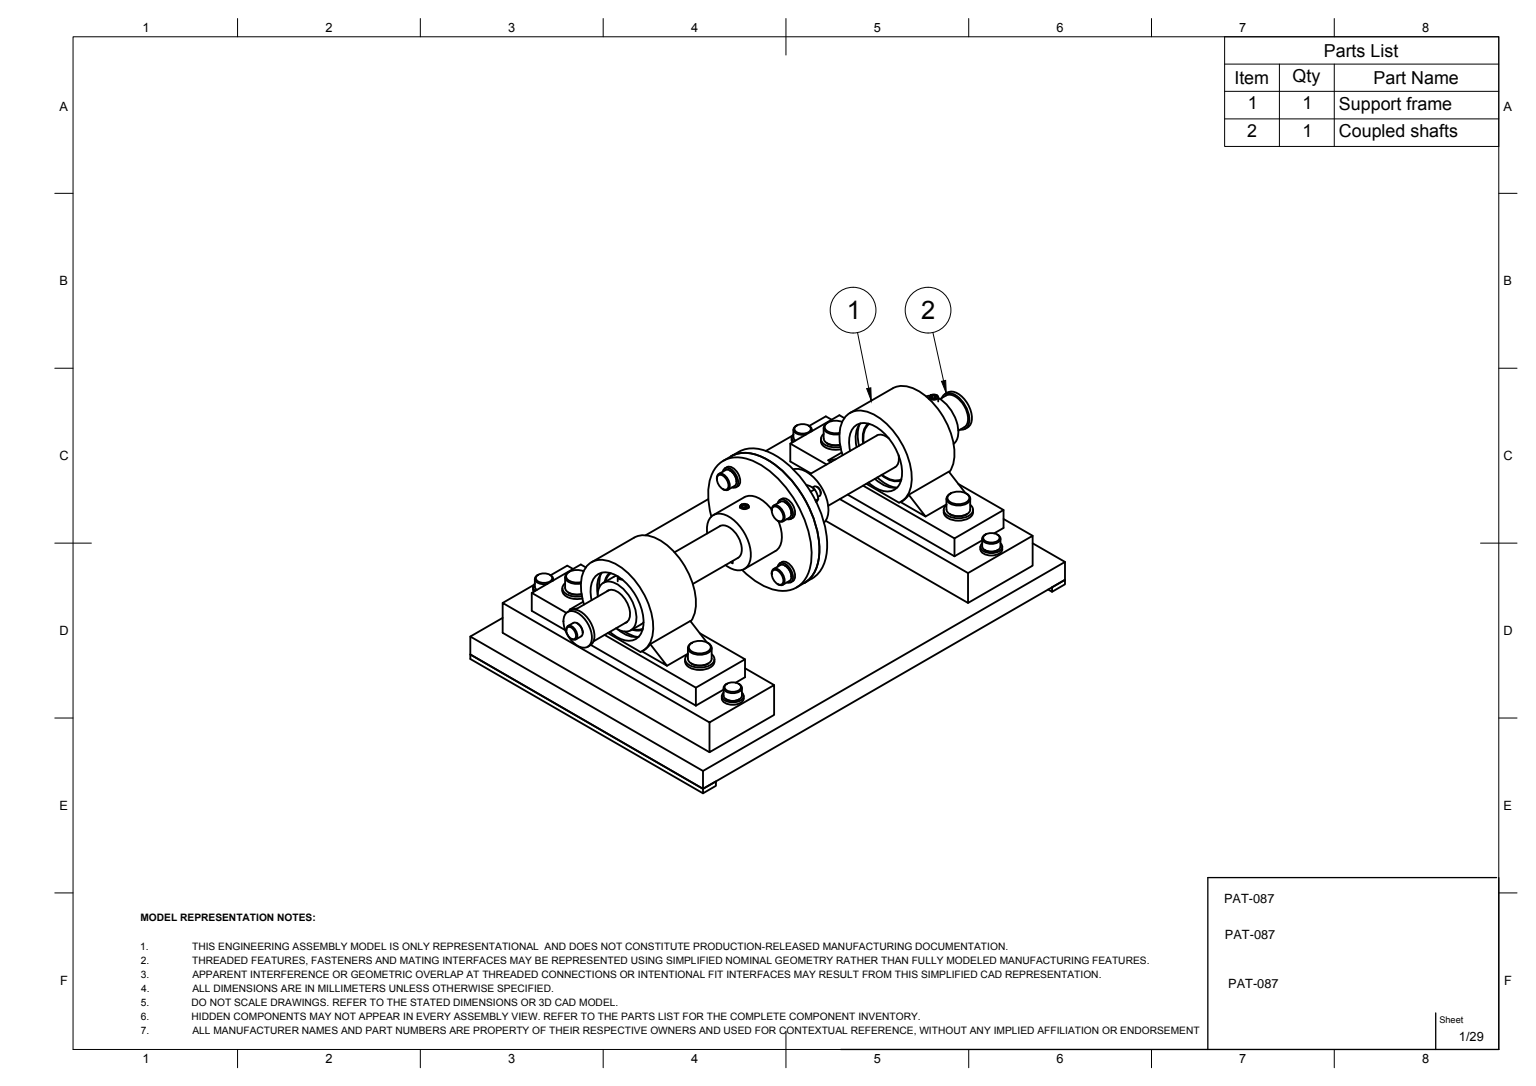
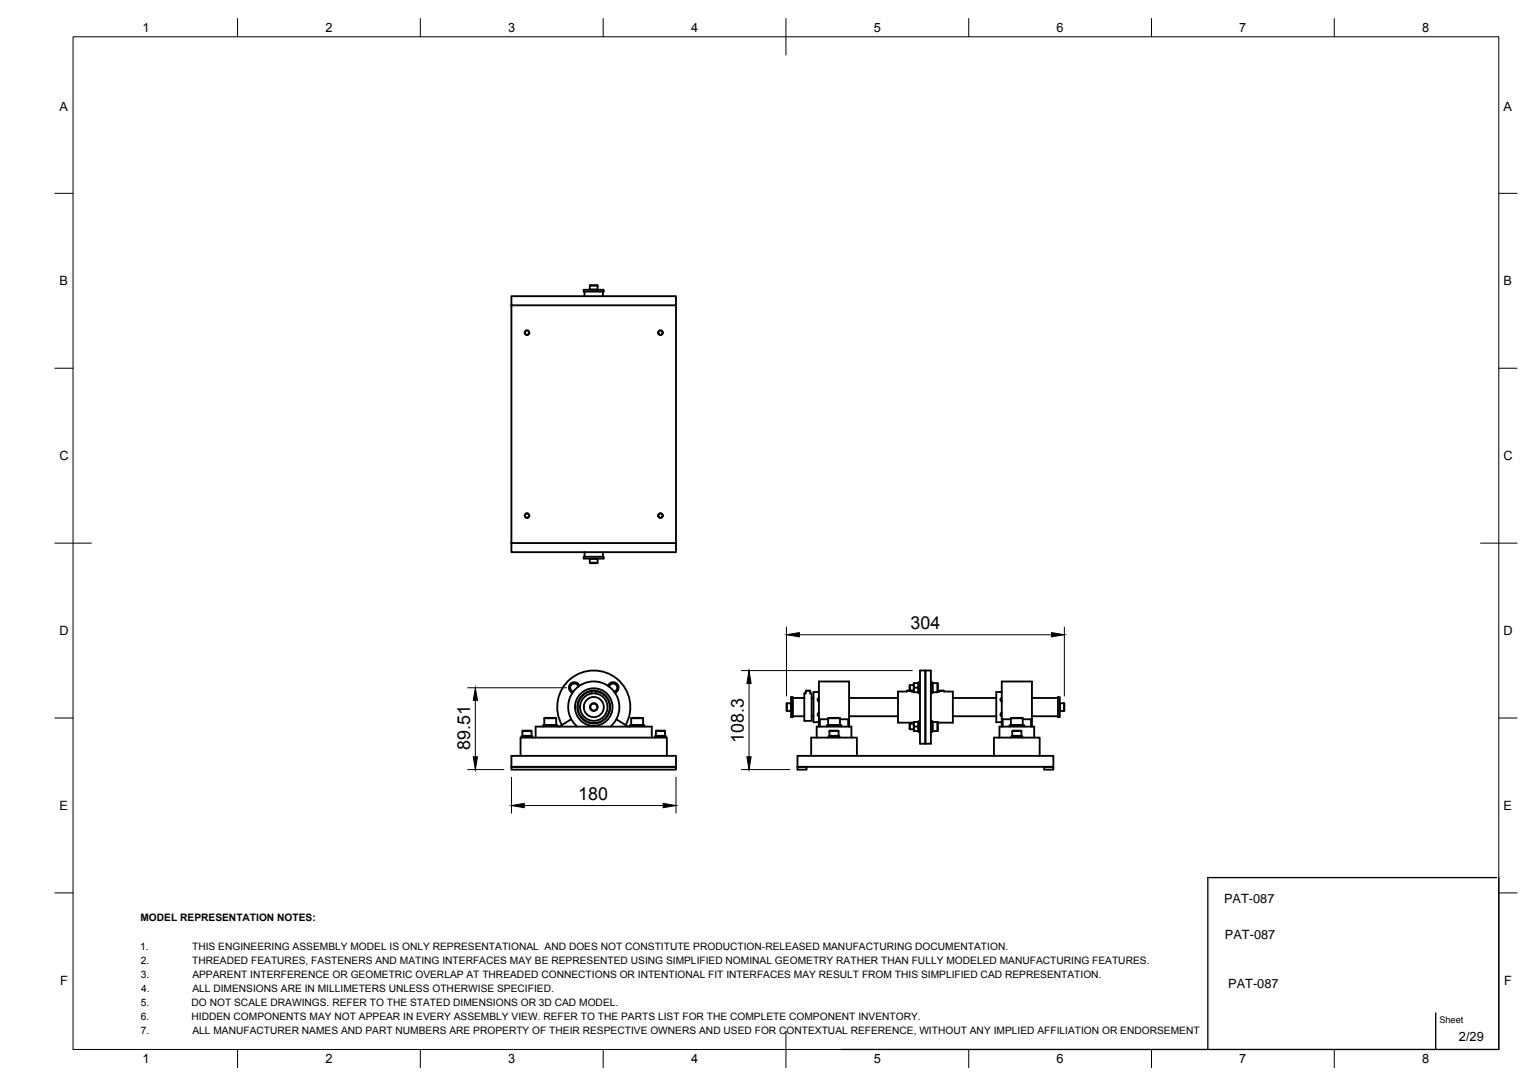
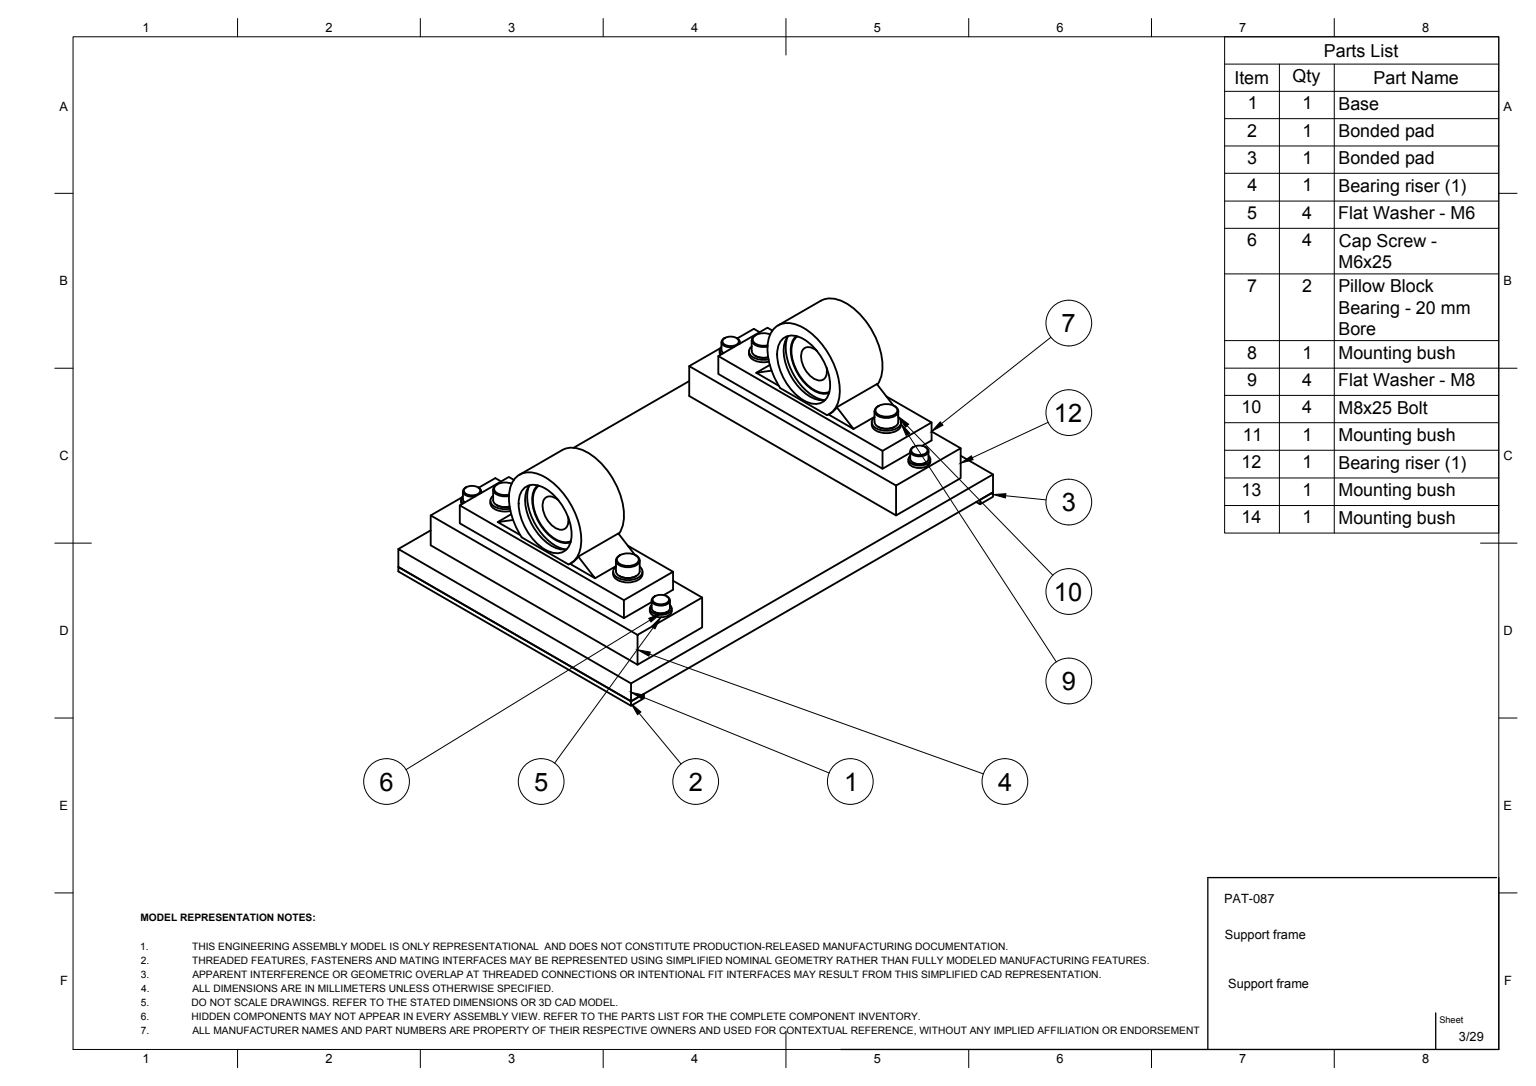
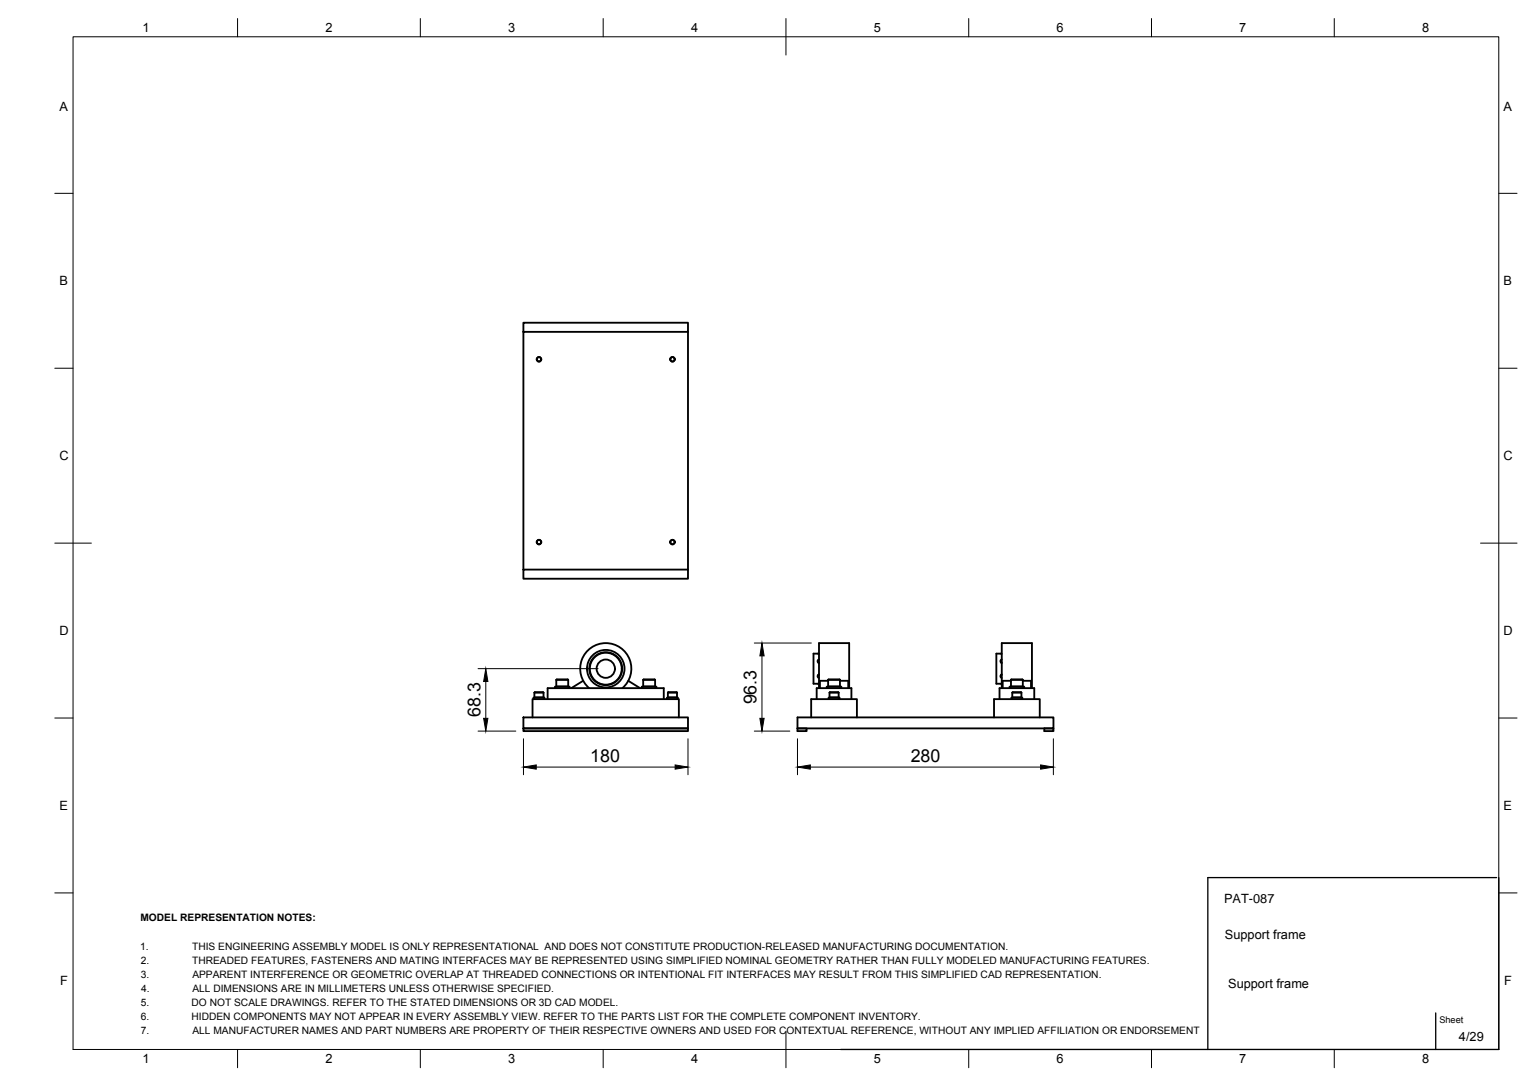
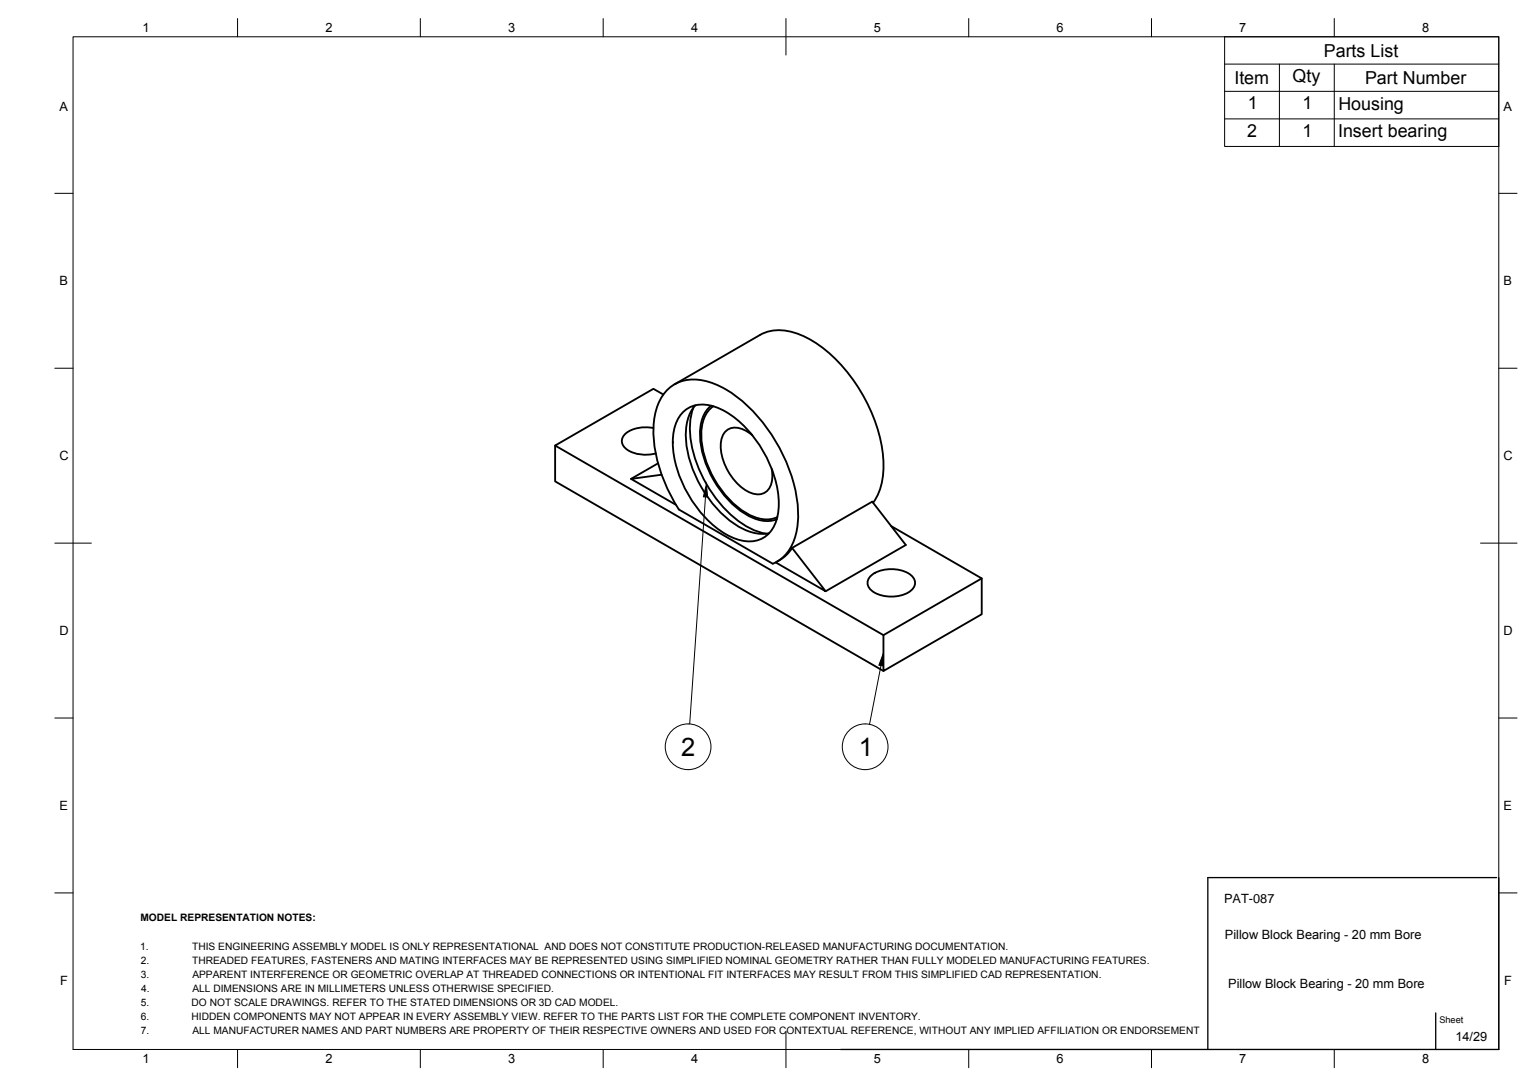
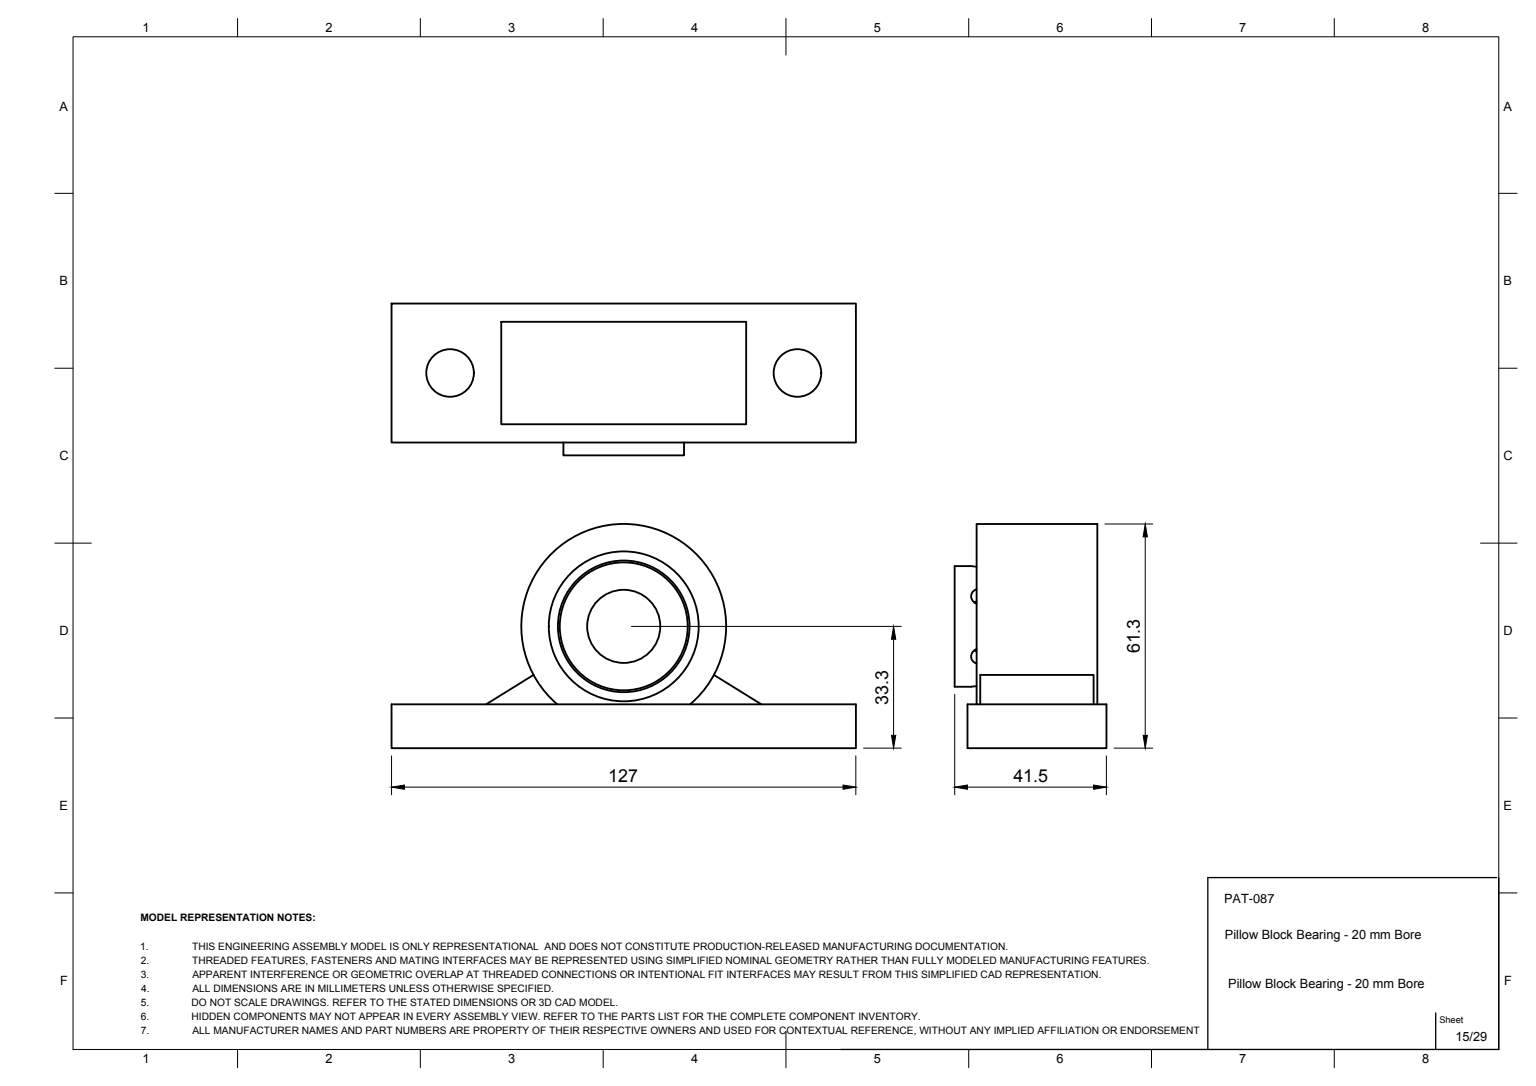
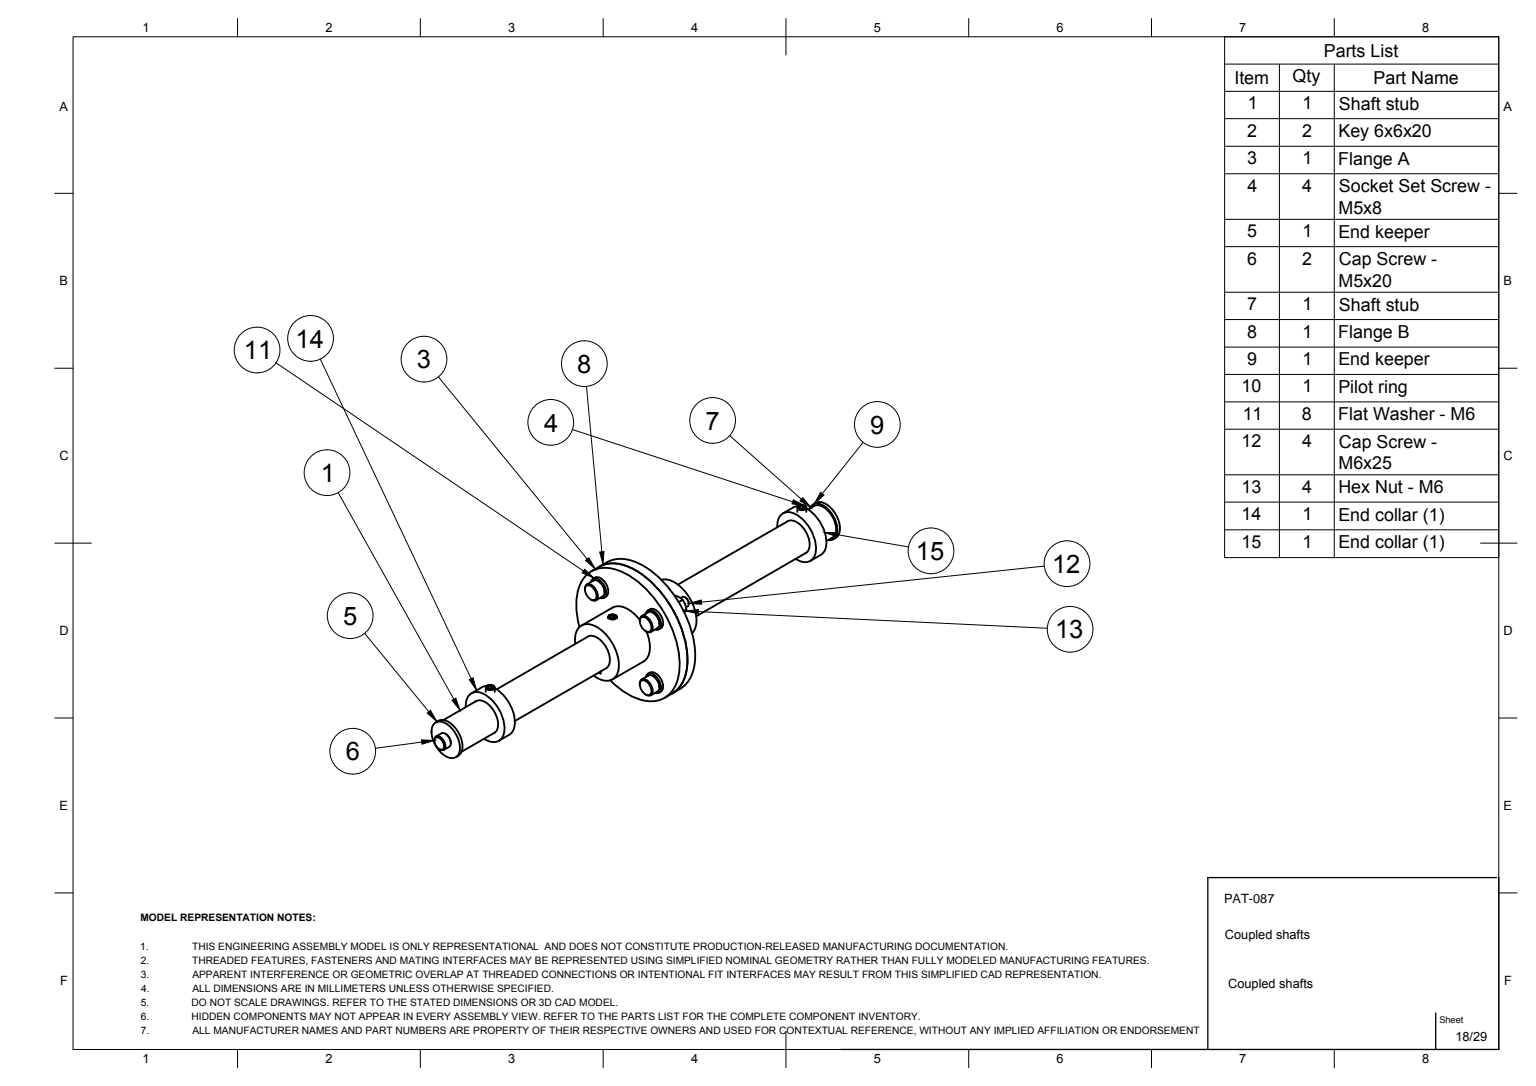
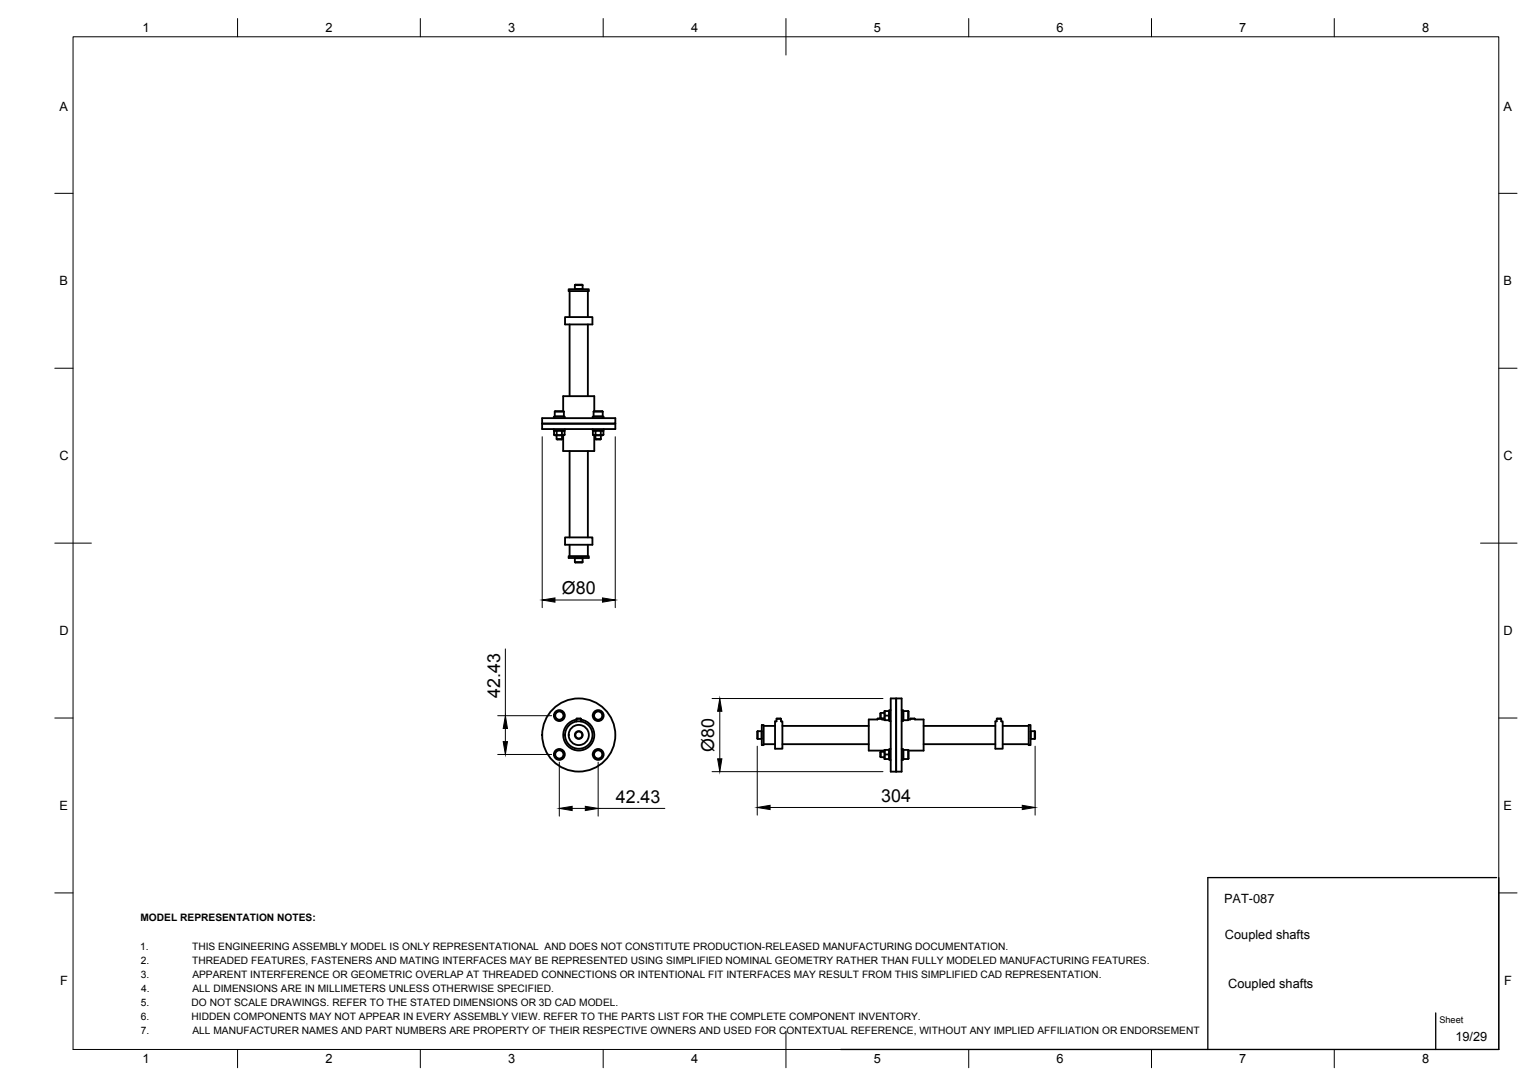
ISO-10303-21;
HEADER;
/* Generated by software containing ST-Developer
 * from STEP Tools, Inc. (www.steptools.com) 
 */

FILE_DESCRIPTION(
/* description */ ('Rigid flange shaft coupling assembly'),
/* implementation_level */ '2;1');

FILE_NAME(
/* name */ 'PAT-087',
/* time_stamp */ '2026-10-27T10:47:16-07:00',
/* author */ (''),
/* organization */ (''),
/* preprocessor_version */ 'ST-DEVELOPER v20.2',
/* originating_system */ 'Autodesk Translation Framework v15.17.0.0',
/* authorisation */ '');

FILE_SCHEMA (('AUTOMOTIVE_DESIGN { 1 0 10303 214 3 1 1 }'));
ENDSEC;

DATA;
#10=MECHANICAL_DESIGN_GEOMETRIC_PRESENTATION_REPRESENTATION('',(#398,#399,
#400,#401,#402,#403,#404,#405,#406,#407,#408,#409,#410,#411,#412,#413,#414,
#415,#416,#417,#418,#419,#420,#421,#422,#423,#424,#425,#426),#9141);
#11=(
BOUNDED_CURVE()
B_SPLINE_CURVE(2,(#8914,#8915,#8916),.UNSPECIFIED.,.F.,.F.)
B_SPLINE_CURVE_WITH_KNOTS((3,3),(0.144988513094728,0.791574906712449),
 .UNSPECIFIED.)
CURVE()
GEOMETRIC_REPRESENTATION_ITEM()
RATIONAL_B_SPLINE_CURVE((1.09282032302755,1.26188021535082,1.09282032302931))
REPRESENTATION_ITEM('')
);
#12=(
BOUNDED_CURVE()
B_SPLINE_CURVE(2,(#8918,#8919,#8920),.UNSPECIFIED.,.F.,.F.)
B_SPLINE_CURVE_WITH_KNOTS((3,3),(0.144988513094728,0.791574906712449),
 .UNSPECIFIED.)
CURVE()
GEOMETRIC_REPRESENTATION_ITEM()
RATIONAL_B_SPLINE_CURVE((1.09282032302755,1.26188021535082,1.09282032302931))
REPRESENTATION_ITEM('')
);
#13=(
BOUNDED_CURVE()
B_SPLINE_CURVE(2,(#8925,#8926,#8927),.UNSPECIFIED.,.F.,.F.)
B_SPLINE_CURVE_WITH_KNOTS((3,3),(0.144988513094728,0.791574906712449),
 .UNSPECIFIED.)
CURVE()
GEOMETRIC_REPRESENTATION_ITEM()
RATIONAL_B_SPLINE_CURVE((1.09282032302755,1.26188021535082,1.09282032302931))
REPRESENTATION_ITEM('')
);
#14=(
BOUNDED_CURVE()
B_SPLINE_CURVE(2,(#8929,#8930,#8931),.UNSPECIFIED.,.F.,.F.)
B_SPLINE_CURVE_WITH_KNOTS((3,3),(0.144988513094728,0.791574906712449),
 .UNSPECIFIED.)
CURVE()
GEOMETRIC_REPRESENTATION_ITEM()
RATIONAL_B_SPLINE_CURVE((1.09282032302755,1.26188021535082,1.09282032302931))
REPRESENTATION_ITEM('')
);
#15=(
BOUNDED_CURVE()
B_SPLINE_CURVE(2,(#8933,#8934,#8935),.UNSPECIFIED.,.F.,.F.)
B_SPLINE_CURVE_WITH_KNOTS((3,3),(0.144988513094728,0.791574906712449),
 .UNSPECIFIED.)
CURVE()
GEOMETRIC_REPRESENTATION_ITEM()
RATIONAL_B_SPLINE_CURVE((1.09282032302755,1.26188021535082,1.09282032302931))
REPRESENTATION_ITEM('')
);
#16=(
BOUNDED_CURVE()
B_SPLINE_CURVE(2,(#8936,#8937,#8938),.UNSPECIFIED.,.F.,.F.)
B_SPLINE_CURVE_WITH_KNOTS((3,3),(0.144988513094728,0.791574906712449),
 .UNSPECIFIED.)
CURVE()
GEOMETRIC_REPRESENTATION_ITEM()
RATIONAL_B_SPLINE_CURVE((1.09282032302755,1.26188021535082,1.09282032302931))
REPRESENTATION_ITEM('')
);
#17=(
BOUNDED_CURVE()
B_SPLINE_CURVE(2,(#8945,#8946,#8947),.UNSPECIFIED.,.F.,.F.)
B_SPLINE_CURVE_WITH_KNOTS((3,3),(0.144988513094728,0.791574906712449),
 .UNSPECIFIED.)
CURVE()
GEOMETRIC_REPRESENTATION_ITEM()
RATIONAL_B_SPLINE_CURVE((1.09282032302755,1.26188021535082,1.09282032302931))
REPRESENTATION_ITEM('')
);
#18=(
BOUNDED_CURVE()
B_SPLINE_CURVE(2,(#8949,#8950,#8951),.UNSPECIFIED.,.F.,.F.)
B_SPLINE_CURVE_WITH_KNOTS((3,3),(0.144988513094727,0.791574906712449),
 .UNSPECIFIED.)
CURVE()
GEOMETRIC_REPRESENTATION_ITEM()
RATIONAL_B_SPLINE_CURVE((1.09282032302755,1.26188021535082,1.09282032302931))
REPRESENTATION_ITEM('')
);
#19=(
BOUNDED_CURVE()
B_SPLINE_CURVE(2,(#8953,#8954,#8955),.UNSPECIFIED.,.F.,.F.)
B_SPLINE_CURVE_WITH_KNOTS((3,3),(0.144988513094728,0.791574906712449),
 .UNSPECIFIED.)
CURVE()
GEOMETRIC_REPRESENTATION_ITEM()
RATIONAL_B_SPLINE_CURVE((1.09282032302755,1.26188021535082,1.09282032302931))
REPRESENTATION_ITEM('')
);
#20=(
BOUNDED_CURVE()
B_SPLINE_CURVE(2,(#8957,#8958,#8959),.UNSPECIFIED.,.F.,.F.)
B_SPLINE_CURVE_WITH_KNOTS((3,3),(0.144988513094728,0.791574906712449),
 .UNSPECIFIED.)
CURVE()
GEOMETRIC_REPRESENTATION_ITEM()
RATIONAL_B_SPLINE_CURVE((1.09282032302755,1.26188021535082,1.09282032302931))
REPRESENTATION_ITEM('')
);
#21=(
BOUNDED_CURVE()
B_SPLINE_CURVE(2,(#8961,#8962,#8963),.UNSPECIFIED.,.F.,.F.)
B_SPLINE_CURVE_WITH_KNOTS((3,3),(0.144988513094728,0.791574906712449),
 .UNSPECIFIED.)
CURVE()
GEOMETRIC_REPRESENTATION_ITEM()
RATIONAL_B_SPLINE_CURVE((1.09282032302755,1.26188021535082,1.09282032302931))
REPRESENTATION_ITEM('')
);
#22=(
BOUNDED_CURVE()
B_SPLINE_CURVE(2,(#8964,#8965,#8966),.UNSPECIFIED.,.F.,.F.)
B_SPLINE_CURVE_WITH_KNOTS((3,3),(0.144988513094727,0.791574906712449),
 .UNSPECIFIED.)
CURVE()
GEOMETRIC_REPRESENTATION_ITEM()
RATIONAL_B_SPLINE_CURVE((1.09282032302755,1.26188021535082,1.09282032302931))
REPRESENTATION_ITEM('')
);
#23=CONICAL_SURFACE('',#5296,0.625,0.785398163397448);
#24=CONICAL_SURFACE('',#5300,0.635,0.785398163397449);
#25=CONICAL_SURFACE('',#5304,0.41,0.463647609000806);
#26=CONICAL_SURFACE('',#5489,0.4,0.785398163397448);
#27=CONICAL_SURFACE('',#5493,0.41,0.785398163397448);
#28=CONICAL_SURFACE('',#5497,0.26,0.463647609000806);
#29=CONICAL_SURFACE('',#5501,0.225,0.785398163397448);
#30=CONICAL_SURFACE('',#5515,0.475,0.785398163397449);
#31=CONICAL_SURFACE('',#5519,0.485,0.785398163397448);
#32=CONICAL_SURFACE('',#5523,0.31,0.463647609000806);
#33=CONICAL_SURFACE('',#5527,0.27,0.785398163397448);
#34=CONICAL_SURFACE('',#5575,0.576175134594813,1.0471975511966);
#35=CONICAL_SURFACE('',#5577,0.576175134594813,1.0471975511966);
#36=CONICAL_SURFACE('',#5600,0.235,0.785398163397448);
#37=CONICAL_SURFACE('',#5604,0.2125,0.785398163397448);
#38=ORIENTED_CLOSED_SHELL('',*,#4765,.F.);
#39=ORIENTED_CLOSED_SHELL('',*,#4778,.F.);
#40=ORIENTED_CLOSED_SHELL('',*,#4780,.F.);
#41=BREP_WITH_VOIDS('Body1',#4766,(#38));
#42=BREP_WITH_VOIDS('Body1',#4777,(#39));
#43=BREP_WITH_VOIDS('Body1',#4779,(#40));
#44=ITEM_DEFINED_TRANSFORMATION($,$,#5203,#5272);
#45=ITEM_DEFINED_TRANSFORMATION($,$,#5244,#5273);
#46=ITEM_DEFINED_TRANSFORMATION($,$,#5095,#5547);
#47=ITEM_DEFINED_TRANSFORMATION($,$,#5114,#5548);
#48=ITEM_DEFINED_TRANSFORMATION($,$,#5121,#5549);
#49=ITEM_DEFINED_TRANSFORMATION($,$,#5128,#5550);
#50=ITEM_DEFINED_TRANSFORMATION($,$,#5147,#5551);
#51=ITEM_DEFINED_TRANSFORMATION($,$,#5156,#5552);
#52=ITEM_DEFINED_TRANSFORMATION($,$,#5165,#5553);
#53=ITEM_DEFINED_TRANSFORMATION($,$,#5184,#5554);
#54=ITEM_DEFINED_TRANSFORMATION($,$,#5193,#5555);
#55=ITEM_DEFINED_TRANSFORMATION($,$,#5538,#5556);
#56=ITEM_DEFINED_TRANSFORMATION($,$,#5512,#5557);
#57=ITEM_DEFINED_TRANSFORMATION($,$,#5538,#5558);
#58=ITEM_DEFINED_TRANSFORMATION($,$,#5512,#5559);
#59=ITEM_DEFINED_TRANSFORMATION($,$,#5202,#5560);
#60=ITEM_DEFINED_TRANSFORMATION($,$,#5274,#5561);
#61=ITEM_DEFINED_TRANSFORMATION($,$,#5283,#5562);
#62=ITEM_DEFINED_TRANSFORMATION($,$,#5274,#5563);
#63=ITEM_DEFINED_TRANSFORMATION($,$,#5283,#5564);
#64=ITEM_DEFINED_TRANSFORMATION($,$,#5538,#5565);
#65=ITEM_DEFINED_TRANSFORMATION($,$,#5512,#5566);
#66=ITEM_DEFINED_TRANSFORMATION($,$,#5538,#5567);
#67=ITEM_DEFINED_TRANSFORMATION($,$,#5512,#5568);
#68=ITEM_DEFINED_TRANSFORMATION($,$,#5202,#5569);
#69=ITEM_DEFINED_TRANSFORMATION($,$,#5274,#5570);
#70=ITEM_DEFINED_TRANSFORMATION($,$,#5283,#5571);
#71=ITEM_DEFINED_TRANSFORMATION($,$,#5274,#5572);
#72=ITEM_DEFINED_TRANSFORMATION($,$,#5283,#5573);
#73=ITEM_DEFINED_TRANSFORMATION($,$,#5308,#5607);
#74=ITEM_DEFINED_TRANSFORMATION($,$,#5325,#5608);
#75=ITEM_DEFINED_TRANSFORMATION($,$,#5363,#5609);
#76=ITEM_DEFINED_TRANSFORMATION($,$,#5372,#5610);
#77=ITEM_DEFINED_TRANSFORMATION($,$,#5389,#5611);
#78=ITEM_DEFINED_TRANSFORMATION($,$,#5427,#5612);
#79=ITEM_DEFINED_TRANSFORMATION($,$,#5436,#5613);
#80=ITEM_DEFINED_TRANSFORMATION($,$,#5445,#5614);
#81=ITEM_DEFINED_TRANSFORMATION($,$,#5460,#5615);
#82=ITEM_DEFINED_TRANSFORMATION($,$,#5475,#5616);
#83=ITEM_DEFINED_TRANSFORMATION($,$,#5590,#5617);
#84=ITEM_DEFINED_TRANSFORMATION($,$,#5486,#5618);
#85=ITEM_DEFINED_TRANSFORMATION($,$,#5475,#5619);
#86=ITEM_DEFINED_TRANSFORMATION($,$,#5590,#5620);
#87=ITEM_DEFINED_TRANSFORMATION($,$,#5486,#5621);
#88=ITEM_DEFINED_TRANSFORMATION($,$,#5538,#5622);
#89=ITEM_DEFINED_TRANSFORMATION($,$,#5512,#5623);
#90=ITEM_DEFINED_TRANSFORMATION($,$,#5538,#5624);
#91=ITEM_DEFINED_TRANSFORMATION($,$,#5574,#5625);
#92=ITEM_DEFINED_TRANSFORMATION($,$,#5538,#5626);
#93=ITEM_DEFINED_TRANSFORMATION($,$,#5512,#5627);
#94=ITEM_DEFINED_TRANSFORMATION($,$,#5538,#5628);
#95=ITEM_DEFINED_TRANSFORMATION($,$,#5574,#5629);
#96=ITEM_DEFINED_TRANSFORMATION($,$,#5538,#5630);
#97=ITEM_DEFINED_TRANSFORMATION($,$,#5512,#5631);
#98=ITEM_DEFINED_TRANSFORMATION($,$,#5538,#5632);
#99=ITEM_DEFINED_TRANSFORMATION($,$,#5574,#5633);
#100=ITEM_DEFINED_TRANSFORMATION($,$,#5538,#5634);
#101=ITEM_DEFINED_TRANSFORMATION($,$,#5512,#5635);
#102=ITEM_DEFINED_TRANSFORMATION($,$,#5538,#5636);
#103=ITEM_DEFINED_TRANSFORMATION($,$,#5574,#5637);
#104=ITEM_DEFINED_TRANSFORMATION($,$,#5590,#5638);
#105=ITEM_DEFINED_TRANSFORMATION($,$,#5590,#5639);
#106=ITEM_DEFINED_TRANSFORMATION($,$,#5094,#5640);
#107=ITEM_DEFINED_TRANSFORMATION($,$,#5307,#5641);
#108=(
REPRESENTATION_RELATIONSHIP($,$,#9286,#9285)
REPRESENTATION_RELATIONSHIP_WITH_TRANSFORMATION(#44)
SHAPE_REPRESENTATION_RELATIONSHIP()
);
#109=(
REPRESENTATION_RELATIONSHIP($,$,#9287,#9285)
REPRESENTATION_RELATIONSHIP_WITH_TRANSFORMATION(#45)
SHAPE_REPRESENTATION_RELATIONSHIP()
);
#110=(
REPRESENTATION_RELATIONSHIP($,$,#9276,#9275)
REPRESENTATION_RELATIONSHIP_WITH_TRANSFORMATION(#46)
SHAPE_REPRESENTATION_RELATIONSHIP()
);
#111=(
REPRESENTATION_RELATIONSHIP($,$,#9277,#9275)
REPRESENTATION_RELATIONSHIP_WITH_TRANSFORMATION(#47)
SHAPE_REPRESENTATION_RELATIONSHIP()
);
#112=(
REPRESENTATION_RELATIONSHIP($,$,#9278,#9275)
REPRESENTATION_RELATIONSHIP_WITH_TRANSFORMATION(#48)
SHAPE_REPRESENTATION_RELATIONSHIP()
);
#113=(
REPRESENTATION_RELATIONSHIP($,$,#9279,#9275)
REPRESENTATION_RELATIONSHIP_WITH_TRANSFORMATION(#49)
SHAPE_REPRESENTATION_RELATIONSHIP()
);
#114=(
REPRESENTATION_RELATIONSHIP($,$,#9280,#9275)
REPRESENTATION_RELATIONSHIP_WITH_TRANSFORMATION(#50)
SHAPE_REPRESENTATION_RELATIONSHIP()
);
#115=(
REPRESENTATION_RELATIONSHIP($,$,#9281,#9275)
REPRESENTATION_RELATIONSHIP_WITH_TRANSFORMATION(#51)
SHAPE_REPRESENTATION_RELATIONSHIP()
);
#116=(
REPRESENTATION_RELATIONSHIP($,$,#9282,#9275)
REPRESENTATION_RELATIONSHIP_WITH_TRANSFORMATION(#52)
SHAPE_REPRESENTATION_RELATIONSHIP()
);
#117=(
REPRESENTATION_RELATIONSHIP($,$,#9283,#9275)
REPRESENTATION_RELATIONSHIP_WITH_TRANSFORMATION(#53)
SHAPE_REPRESENTATION_RELATIONSHIP()
);
#118=(
REPRESENTATION_RELATIONSHIP($,$,#9284,#9275)
REPRESENTATION_RELATIONSHIP_WITH_TRANSFORMATION(#54)
SHAPE_REPRESENTATION_RELATIONSHIP()
);
#119=(
REPRESENTATION_RELATIONSHIP($,$,#9303,#9275)
REPRESENTATION_RELATIONSHIP_WITH_TRANSFORMATION(#55)
SHAPE_REPRESENTATION_RELATIONSHIP()
);
#120=(
REPRESENTATION_RELATIONSHIP($,$,#9302,#9275)
REPRESENTATION_RELATIONSHIP_WITH_TRANSFORMATION(#56)
SHAPE_REPRESENTATION_RELATIONSHIP()
);
#121=(
REPRESENTATION_RELATIONSHIP($,$,#9303,#9275)
REPRESENTATION_RELATIONSHIP_WITH_TRANSFORMATION(#57)
SHAPE_REPRESENTATION_RELATIONSHIP()
);
#122=(
REPRESENTATION_RELATIONSHIP($,$,#9302,#9275)
REPRESENTATION_RELATIONSHIP_WITH_TRANSFORMATION(#58)
SHAPE_REPRESENTATION_RELATIONSHIP()
);
#123=(
REPRESENTATION_RELATIONSHIP($,$,#9285,#9275)
REPRESENTATION_RELATIONSHIP_WITH_TRANSFORMATION(#59)
SHAPE_REPRESENTATION_RELATIONSHIP()
);
#124=(
REPRESENTATION_RELATIONSHIP($,$,#9288,#9275)
REPRESENTATION_RELATIONSHIP_WITH_TRANSFORMATION(#60)
SHAPE_REPRESENTATION_RELATIONSHIP()
);
#125=(
REPRESENTATION_RELATIONSHIP($,$,#9289,#9275)
REPRESENTATION_RELATIONSHIP_WITH_TRANSFORMATION(#61)
SHAPE_REPRESENTATION_RELATIONSHIP()
);
#126=(
REPRESENTATION_RELATIONSHIP($,$,#9288,#9275)
REPRESENTATION_RELATIONSHIP_WITH_TRANSFORMATION(#62)
SHAPE_REPRESENTATION_RELATIONSHIP()
);
#127=(
REPRESENTATION_RELATIONSHIP($,$,#9289,#9275)
REPRESENTATION_RELATIONSHIP_WITH_TRANSFORMATION(#63)
SHAPE_REPRESENTATION_RELATIONSHIP()
);
#128=(
REPRESENTATION_RELATIONSHIP($,$,#9303,#9275)
REPRESENTATION_RELATIONSHIP_WITH_TRANSFORMATION(#64)
SHAPE_REPRESENTATION_RELATIONSHIP()
);
#129=(
REPRESENTATION_RELATIONSHIP($,$,#9302,#9275)
REPRESENTATION_RELATIONSHIP_WITH_TRANSFORMATION(#65)
SHAPE_REPRESENTATION_RELATIONSHIP()
);
#130=(
REPRESENTATION_RELATIONSHIP($,$,#9303,#9275)
REPRESENTATION_RELATIONSHIP_WITH_TRANSFORMATION(#66)
SHAPE_REPRESENTATION_RELATIONSHIP()
);
#131=(
REPRESENTATION_RELATIONSHIP($,$,#9302,#9275)
REPRESENTATION_RELATIONSHIP_WITH_TRANSFORMATION(#67)
SHAPE_REPRESENTATION_RELATIONSHIP()
);
#132=(
REPRESENTATION_RELATIONSHIP($,$,#9285,#9275)
REPRESENTATION_RELATIONSHIP_WITH_TRANSFORMATION(#68)
SHAPE_REPRESENTATION_RELATIONSHIP()
);
#133=(
REPRESENTATION_RELATIONSHIP($,$,#9288,#9275)
REPRESENTATION_RELATIONSHIP_WITH_TRANSFORMATION(#69)
SHAPE_REPRESENTATION_RELATIONSHIP()
);
#134=(
REPRESENTATION_RELATIONSHIP($,$,#9289,#9275)
REPRESENTATION_RELATIONSHIP_WITH_TRANSFORMATION(#70)
SHAPE_REPRESENTATION_RELATIONSHIP()
);
#135=(
REPRESENTATION_RELATIONSHIP($,$,#9288,#9275)
REPRESENTATION_RELATIONSHIP_WITH_TRANSFORMATION(#71)
SHAPE_REPRESENTATION_RELATIONSHIP()
);
#136=(
REPRESENTATION_RELATIONSHIP($,$,#9289,#9275)
REPRESENTATION_RELATIONSHIP_WITH_TRANSFORMATION(#72)
SHAPE_REPRESENTATION_RELATIONSHIP()
);
#137=(
REPRESENTATION_RELATIONSHIP($,$,#9291,#9290)
REPRESENTATION_RELATIONSHIP_WITH_TRANSFORMATION(#73)
SHAPE_REPRESENTATION_RELATIONSHIP()
);
#138=(
REPRESENTATION_RELATIONSHIP($,$,#9292,#9290)
REPRESENTATION_RELATIONSHIP_WITH_TRANSFORMATION(#74)
SHAPE_REPRESENTATION_RELATIONSHIP()
);
#139=(
REPRESENTATION_RELATIONSHIP($,$,#9293,#9290)
REPRESENTATION_RELATIONSHIP_WITH_TRANSFORMATION(#75)
SHAPE_REPRESENTATION_RELATIONSHIP()
);
#140=(
REPRESENTATION_RELATIONSHIP($,$,#9294,#9290)
REPRESENTATION_RELATIONSHIP_WITH_TRANSFORMATION(#76)
SHAPE_REPRESENTATION_RELATIONSHIP()
);
#141=(
REPRESENTATION_RELATIONSHIP($,$,#9295,#9290)
REPRESENTATION_RELATIONSHIP_WITH_TRANSFORMATION(#77)
SHAPE_REPRESENTATION_RELATIONSHIP()
);
#142=(
REPRESENTATION_RELATIONSHIP($,$,#9296,#9290)
REPRESENTATION_RELATIONSHIP_WITH_TRANSFORMATION(#78)
SHAPE_REPRESENTATION_RELATIONSHIP()
);
#143=(
REPRESENTATION_RELATIONSHIP($,$,#9297,#9290)
REPRESENTATION_RELATIONSHIP_WITH_TRANSFORMATION(#79)
SHAPE_REPRESENTATION_RELATIONSHIP()
);
#144=(
REPRESENTATION_RELATIONSHIP($,$,#9298,#9290)
REPRESENTATION_RELATIONSHIP_WITH_TRANSFORMATION(#80)
SHAPE_REPRESENTATION_RELATIONSHIP()
);
#145=(
REPRESENTATION_RELATIONSHIP($,$,#9299,#9290)
REPRESENTATION_RELATIONSHIP_WITH_TRANSFORMATION(#81)
SHAPE_REPRESENTATION_RELATIONSHIP()
);
#146=(
REPRESENTATION_RELATIONSHIP($,$,#9300,#9290)
REPRESENTATION_RELATIONSHIP_WITH_TRANSFORMATION(#82)
SHAPE_REPRESENTATION_RELATIONSHIP()
);
#147=(
REPRESENTATION_RELATIONSHIP($,$,#9305,#9290)
REPRESENTATION_RELATIONSHIP_WITH_TRANSFORMATION(#83)
SHAPE_REPRESENTATION_RELATIONSHIP()
);
#148=(
REPRESENTATION_RELATIONSHIP($,$,#9301,#9290)
REPRESENTATION_RELATIONSHIP_WITH_TRANSFORMATION(#84)
SHAPE_REPRESENTATION_RELATIONSHIP()
);
#149=(
REPRESENTATION_RELATIONSHIP($,$,#9300,#9290)
REPRESENTATION_RELATIONSHIP_WITH_TRANSFORMATION(#85)
SHAPE_REPRESENTATION_RELATIONSHIP()
);
#150=(
REPRESENTATION_RELATIONSHIP($,$,#9305,#9290)
REPRESENTATION_RELATIONSHIP_WITH_TRANSFORMATION(#86)
SHAPE_REPRESENTATION_RELATIONSHIP()
);
#151=(
REPRESENTATION_RELATIONSHIP($,$,#9301,#9290)
REPRESENTATION_RELATIONSHIP_WITH_TRANSFORMATION(#87)
SHAPE_REPRESENTATION_RELATIONSHIP()
);
#152=(
REPRESENTATION_RELATIONSHIP($,$,#9303,#9290)
REPRESENTATION_RELATIONSHIP_WITH_TRANSFORMATION(#88)
SHAPE_REPRESENTATION_RELATIONSHIP()
);
#153=(
REPRESENTATION_RELATIONSHIP($,$,#9302,#9290)
REPRESENTATION_RELATIONSHIP_WITH_TRANSFORMATION(#89)
SHAPE_REPRESENTATION_RELATIONSHIP()
);
#154=(
REPRESENTATION_RELATIONSHIP($,$,#9303,#9290)
REPRESENTATION_RELATIONSHIP_WITH_TRANSFORMATION(#90)
SHAPE_REPRESENTATION_RELATIONSHIP()
);
#155=(
REPRESENTATION_RELATIONSHIP($,$,#9304,#9290)
REPRESENTATION_RELATIONSHIP_WITH_TRANSFORMATION(#91)
SHAPE_REPRESENTATION_RELATIONSHIP()
);
#156=(
REPRESENTATION_RELATIONSHIP($,$,#9303,#9290)
REPRESENTATION_RELATIONSHIP_WITH_TRANSFORMATION(#92)
SHAPE_REPRESENTATION_RELATIONSHIP()
);
#157=(
REPRESENTATION_RELATIONSHIP($,$,#9302,#9290)
REPRESENTATION_RELATIONSHIP_WITH_TRANSFORMATION(#93)
SHAPE_REPRESENTATION_RELATIONSHIP()
);
#158=(
REPRESENTATION_RELATIONSHIP($,$,#9303,#9290)
REPRESENTATION_RELATIONSHIP_WITH_TRANSFORMATION(#94)
SHAPE_REPRESENTATION_RELATIONSHIP()
);
#159=(
REPRESENTATION_RELATIONSHIP($,$,#9304,#9290)
REPRESENTATION_RELATIONSHIP_WITH_TRANSFORMATION(#95)
SHAPE_REPRESENTATION_RELATIONSHIP()
);
#160=(
REPRESENTATION_RELATIONSHIP($,$,#9303,#9290)
REPRESENTATION_RELATIONSHIP_WITH_TRANSFORMATION(#96)
SHAPE_REPRESENTATION_RELATIONSHIP()
);
#161=(
REPRESENTATION_RELATIONSHIP($,$,#9302,#9290)
REPRESENTATION_RELATIONSHIP_WITH_TRANSFORMATION(#97)
SHAPE_REPRESENTATION_RELATIONSHIP()
);
#162=(
REPRESENTATION_RELATIONSHIP($,$,#9303,#9290)
REPRESENTATION_RELATIONSHIP_WITH_TRANSFORMATION(#98)
SHAPE_REPRESENTATION_RELATIONSHIP()
);
#163=(
REPRESENTATION_RELATIONSHIP($,$,#9304,#9290)
REPRESENTATION_RELATIONSHIP_WITH_TRANSFORMATION(#99)
SHAPE_REPRESENTATION_RELATIONSHIP()
);
#164=(
REPRESENTATION_RELATIONSHIP($,$,#9303,#9290)
REPRESENTATION_RELATIONSHIP_WITH_TRANSFORMATION(#100)
SHAPE_REPRESENTATION_RELATIONSHIP()
);
#165=(
REPRESENTATION_RELATIONSHIP($,$,#9302,#9290)
REPRESENTATION_RELATIONSHIP_WITH_TRANSFORMATION(#101)
SHAPE_REPRESENTATION_RELATIONSHIP()
);
#166=(
REPRESENTATION_RELATIONSHIP($,$,#9303,#9290)
REPRESENTATION_RELATIONSHIP_WITH_TRANSFORMATION(#102)
SHAPE_REPRESENTATION_RELATIONSHIP()
);
#167=(
REPRESENTATION_RELATIONSHIP($,$,#9304,#9290)
REPRESENTATION_RELATIONSHIP_WITH_TRANSFORMATION(#103)
SHAPE_REPRESENTATION_RELATIONSHIP()
);
#168=(
REPRESENTATION_RELATIONSHIP($,$,#9305,#9290)
REPRESENTATION_RELATIONSHIP_WITH_TRANSFORMATION(#104)
SHAPE_REPRESENTATION_RELATIONSHIP()
);
#169=(
REPRESENTATION_RELATIONSHIP($,$,#9305,#9290)
REPRESENTATION_RELATIONSHIP_WITH_TRANSFORMATION(#105)
SHAPE_REPRESENTATION_RELATIONSHIP()
);
#170=(
REPRESENTATION_RELATIONSHIP($,$,#9275,#9274)
REPRESENTATION_RELATIONSHIP_WITH_TRANSFORMATION(#106)
SHAPE_REPRESENTATION_RELATIONSHIP()
);
#171=(
REPRESENTATION_RELATIONSHIP($,$,#9290,#9274)
REPRESENTATION_RELATIONSHIP_WITH_TRANSFORMATION(#107)
SHAPE_REPRESENTATION_RELATIONSHIP()
);
#172=CONTEXT_DEPENDENT_SHAPE_REPRESENTATION(#108,#9192);
#173=CONTEXT_DEPENDENT_SHAPE_REPRESENTATION(#109,#9193);
#174=CONTEXT_DEPENDENT_SHAPE_REPRESENTATION(#110,#9210);
#175=CONTEXT_DEPENDENT_SHAPE_REPRESENTATION(#111,#9211);
#176=CONTEXT_DEPENDENT_SHAPE_REPRESENTATION(#112,#9212);
#177=CONTEXT_DEPENDENT_SHAPE_REPRESENTATION(#113,#9213);
#178=CONTEXT_DEPENDENT_SHAPE_REPRESENTATION(#114,#9214);
#179=CONTEXT_DEPENDENT_SHAPE_REPRESENTATION(#115,#9215);
#180=CONTEXT_DEPENDENT_SHAPE_REPRESENTATION(#116,#9216);
#181=CONTEXT_DEPENDENT_SHAPE_REPRESENTATION(#117,#9217);
#182=CONTEXT_DEPENDENT_SHAPE_REPRESENTATION(#118,#9218);
#183=CONTEXT_DEPENDENT_SHAPE_REPRESENTATION(#119,#9219);
#184=CONTEXT_DEPENDENT_SHAPE_REPRESENTATION(#120,#9220);
#185=CONTEXT_DEPENDENT_SHAPE_REPRESENTATION(#121,#9221);
#186=CONTEXT_DEPENDENT_SHAPE_REPRESENTATION(#122,#9222);
#187=CONTEXT_DEPENDENT_SHAPE_REPRESENTATION(#123,#9223);
#188=CONTEXT_DEPENDENT_SHAPE_REPRESENTATION(#124,#9224);
#189=CONTEXT_DEPENDENT_SHAPE_REPRESENTATION(#125,#9225);
#190=CONTEXT_DEPENDENT_SHAPE_REPRESENTATION(#126,#9226);
#191=CONTEXT_DEPENDENT_SHAPE_REPRESENTATION(#127,#9227);
#192=CONTEXT_DEPENDENT_SHAPE_REPRESENTATION(#128,#9228);
#193=CONTEXT_DEPENDENT_SHAPE_REPRESENTATION(#129,#9229);
#194=CONTEXT_DEPENDENT_SHAPE_REPRESENTATION(#130,#9230);
#195=CONTEXT_DEPENDENT_SHAPE_REPRESENTATION(#131,#9231);
#196=CONTEXT_DEPENDENT_SHAPE_REPRESENTATION(#132,#9232);
#197=CONTEXT_DEPENDENT_SHAPE_REPRESENTATION(#133,#9233);
#198=CONTEXT_DEPENDENT_SHAPE_REPRESENTATION(#134,#9234);
#199=CONTEXT_DEPENDENT_SHAPE_REPRESENTATION(#135,#9235);
#200=CONTEXT_DEPENDENT_SHAPE_REPRESENTATION(#136,#9236);
#201=CONTEXT_DEPENDENT_SHAPE_REPRESENTATION(#137,#9239);
#202=CONTEXT_DEPENDENT_SHAPE_REPRESENTATION(#138,#9240);
#203=CONTEXT_DEPENDENT_SHAPE_REPRESENTATION(#139,#9241);
#204=CONTEXT_DEPENDENT_SHAPE_REPRESENTATION(#140,#9242);
#205=CONTEXT_DEPENDENT_SHAPE_REPRESENTATION(#141,#9243);
#206=CONTEXT_DEPENDENT_SHAPE_REPRESENTATION(#142,#9244);
#207=CONTEXT_DEPENDENT_SHAPE_REPRESENTATION(#143,#9245);
#208=CONTEXT_DEPENDENT_SHAPE_REPRESENTATION(#144,#9246);
#209=CONTEXT_DEPENDENT_SHAPE_REPRESENTATION(#145,#9247);
#210=CONTEXT_DEPENDENT_SHAPE_REPRESENTATION(#146,#9248);
#211=CONTEXT_DEPENDENT_SHAPE_REPRESENTATION(#147,#9249);
#212=CONTEXT_DEPENDENT_SHAPE_REPRESENTATION(#148,#9250);
#213=CONTEXT_DEPENDENT_SHAPE_REPRESENTATION(#149,#9251);
#214=CONTEXT_DEPENDENT_SHAPE_REPRESENTATION(#150,#9252);
#215=CONTEXT_DEPENDENT_SHAPE_REPRESENTATION(#151,#9253);
#216=CONTEXT_DEPENDENT_SHAPE_REPRESENTATION(#152,#9254);
#217=CONTEXT_DEPENDENT_SHAPE_REPRESENTATION(#153,#9255);
#218=CONTEXT_DEPENDENT_SHAPE_REPRESENTATION(#154,#9256);
#219=CONTEXT_DEPENDENT_SHAPE_REPRESENTATION(#155,#9257);
#220=CONTEXT_DEPENDENT_SHAPE_REPRESENTATION(#156,#9258);
#221=CONTEXT_DEPENDENT_SHAPE_REPRESENTATION(#157,#9259);
#222=CONTEXT_DEPENDENT_SHAPE_REPRESENTATION(#158,#9260);
#223=CONTEXT_DEPENDENT_SHAPE_REPRESENTATION(#159,#9261);
#224=CONTEXT_DEPENDENT_SHAPE_REPRESENTATION(#160,#9262);
#225=CONTEXT_DEPENDENT_SHAPE_REPRESENTATION(#161,#9263);
#226=CONTEXT_DEPENDENT_SHAPE_REPRESENTATION(#162,#9264);
#227=CONTEXT_DEPENDENT_SHAPE_REPRESENTATION(#163,#9265);
#228=CONTEXT_DEPENDENT_SHAPE_REPRESENTATION(#164,#9266);
#229=CONTEXT_DEPENDENT_SHAPE_REPRESENTATION(#165,#9267);
#230=CONTEXT_DEPENDENT_SHAPE_REPRESENTATION(#166,#9268);
#231=CONTEXT_DEPENDENT_SHAPE_REPRESENTATION(#167,#9269);
#232=CONTEXT_DEPENDENT_SHAPE_REPRESENTATION(#168,#9270);
#233=CONTEXT_DEPENDENT_SHAPE_REPRESENTATION(#169,#9271);
#234=CONTEXT_DEPENDENT_SHAPE_REPRESENTATION(#170,#9272);
#235=CONTEXT_DEPENDENT_SHAPE_REPRESENTATION(#171,#9273);
#236=NEXT_ASSEMBLY_USAGE_OCCURRENCE('Housing:1','Housing:1','Housing:1',
#9318,#9319,'Housing:1');
#237=NEXT_ASSEMBLY_USAGE_OCCURRENCE('Insert bearing:1',
'Insert bearing:1','Insert bearing:1',#9318,#9320,'Insert bearing:1');
#238=NEXT_ASSEMBLY_USAGE_OCCURRENCE('Base:1','Base:1','Base:1',#9308,#9309,
'Base:1');
#239=NEXT_ASSEMBLY_USAGE_OCCURRENCE('Bonded pad:1','Bonded pad:1',
'Bonded pad:1',#9308,#9310,'Bonded pad:1');
#240=NEXT_ASSEMBLY_USAGE_OCCURRENCE('Bonded pad (1):1',
'Bonded pad (1):1','Bonded pad (1):1',#9308,#9311,'Bonded pad (1):1');
#241=NEXT_ASSEMBLY_USAGE_OCCURRENCE('Bearing riser:1','Bearing riser:1',
'Bearing riser:1',#9308,#9312,'Bearing riser:1');
#242=NEXT_ASSEMBLY_USAGE_OCCURRENCE('Mounting bush:1','Mounting bush:1',
'Mounting bush:1',#9308,#9313,'Mounting bush:1');
#243=NEXT_ASSEMBLY_USAGE_OCCURRENCE('Mounting bush (1):1',
'Mounting bush (1):1','Mounting bush (1):1',#9308,#9314,
'Mounting bush (1):1');
#244=NEXT_ASSEMBLY_USAGE_OCCURRENCE('Bearing riser (1):1',
'Bearing riser (1):1','Bearing riser (1):1',#9308,#9315,
'Bearing riser (1):1');
#245=NEXT_ASSEMBLY_USAGE_OCCURRENCE('Mounting bush (2):1',
'Mounting bush (2):1','Mounting bush (2):1',#9308,#9316,
'Mounting bush (2):1');
#246=NEXT_ASSEMBLY_USAGE_OCCURRENCE('Mounting bush (3):1',
'Mounting bush (3):1','Mounting bush (3):1',#9308,#9317,
'Mounting bush (3):1');
#247=NEXT_ASSEMBLY_USAGE_OCCURRENCE('Flat Washer - M6:2',
'Flat Washer - M6:2','Flat Washer - M6:2',#9308,#9336,
'Flat Washer - M6:2');
#248=NEXT_ASSEMBLY_USAGE_OCCURRENCE('Cap Screw - M6x25:2',
'Cap Screw - M6x25:2','Cap Screw - M6x25:2',#9308,#9335,
'Cap Screw - M6x25:2');
#249=NEXT_ASSEMBLY_USAGE_OCCURRENCE('Flat Washer - M6:3',
'Flat Washer - M6:3','Flat Washer - M6:3',#9308,#9336,
'Flat Washer - M6:3');
#250=NEXT_ASSEMBLY_USAGE_OCCURRENCE('Cap Screw - M6x25:3',
'Cap Screw - M6x25:3','Cap Screw - M6x25:3',#9308,#9335,
'Cap Screw - M6x25:3');
#251=NEXT_ASSEMBLY_USAGE_OCCURRENCE(
'Pillow Block Bearing - 20 mm Bore:2',
'Pillow Block Bearing - 20 mm Bore:2',
'Pillow Block Bearing - 20 mm Bore:2',#9308,#9318,
'Pillow Block Bearing - 20 mm Bore:2');
#252=NEXT_ASSEMBLY_USAGE_OCCURRENCE('Flat Washer - M8:2',
'Flat Washer - M8:2','Flat Washer - M8:2',#9308,#9321,
'Flat Washer - M8:2');
#253=NEXT_ASSEMBLY_USAGE_OCCURRENCE('M8x25 Bolt:2','M8x25 Bolt:2',
'M8x25 Bolt:2',#9308,#9322,'M8x25 Bolt:2');
#254=NEXT_ASSEMBLY_USAGE_OCCURRENCE('Flat Washer - M8:3',
'Flat Washer - M8:3','Flat Washer - M8:3',#9308,#9321,
'Flat Washer - M8:3');
#255=NEXT_ASSEMBLY_USAGE_OCCURRENCE('M8x25 Bolt:3','M8x25 Bolt:3',
'M8x25 Bolt:3',#9308,#9322,'M8x25 Bolt:3');
#256=NEXT_ASSEMBLY_USAGE_OCCURRENCE('Flat Washer - M6:4',
'Flat Washer - M6:4','Flat Washer - M6:4',#9308,#9336,
'Flat Washer - M6:4');
#257=NEXT_ASSEMBLY_USAGE_OCCURRENCE('Cap Screw - M6x25:4',
'Cap Screw - M6x25:4','Cap Screw - M6x25:4',#9308,#9335,
'Cap Screw - M6x25:4');
#258=NEXT_ASSEMBLY_USAGE_OCCURRENCE('Flat Washer - M6:5',
'Flat Washer - M6:5','Flat Washer - M6:5',#9308,#9336,
'Flat Washer - M6:5');
#259=NEXT_ASSEMBLY_USAGE_OCCURRENCE('Cap Screw - M6x25:5',
'Cap Screw - M6x25:5','Cap Screw - M6x25:5',#9308,#9335,
'Cap Screw - M6x25:5');
#260=NEXT_ASSEMBLY_USAGE_OCCURRENCE(
'Pillow Block Bearing - 20 mm Bore:3',
'Pillow Block Bearing - 20 mm Bore:3',
'Pillow Block Bearing - 20 mm Bore:3',#9308,#9318,
'Pillow Block Bearing - 20 mm Bore:3');
#261=NEXT_ASSEMBLY_USAGE_OCCURRENCE('Flat Washer - M8:4',
'Flat Washer - M8:4','Flat Washer - M8:4',#9308,#9321,
'Flat Washer - M8:4');
#262=NEXT_ASSEMBLY_USAGE_OCCURRENCE('M8x25 Bolt:4','M8x25 Bolt:4',
'M8x25 Bolt:4',#9308,#9322,'M8x25 Bolt:4');
#263=NEXT_ASSEMBLY_USAGE_OCCURRENCE('Flat Washer - M8:5',
'Flat Washer - M8:5','Flat Washer - M8:5',#9308,#9321,
'Flat Washer - M8:5');
#264=NEXT_ASSEMBLY_USAGE_OCCURRENCE('M8x25 Bolt:5','M8x25 Bolt:5',
'M8x25 Bolt:5',#9308,#9322,'M8x25 Bolt:5');
#265=NEXT_ASSEMBLY_USAGE_OCCURRENCE('Shaft stub:1','Shaft stub:1',
'Shaft stub:1',#9323,#9324,'Shaft stub:1');
#266=NEXT_ASSEMBLY_USAGE_OCCURRENCE('Flange A:1','Flange A:1',
'Flange A:1',#9323,#9325,'Flange A:1');
#267=NEXT_ASSEMBLY_USAGE_OCCURRENCE('End keeper:1','End keeper:1',
'End keeper:1',#9323,#9326,'End keeper:1');
#268=NEXT_ASSEMBLY_USAGE_OCCURRENCE('Shaft stub (1):1',
'Shaft stub (1):1','Shaft stub (1):1',#9323,#9327,'Shaft stub (1):1');
#269=NEXT_ASSEMBLY_USAGE_OCCURRENCE('Flange B:1','Flange B:1',
'Flange B:1',#9323,#9328,'Flange B:1');
#270=NEXT_ASSEMBLY_USAGE_OCCURRENCE('End keeper (1):1',
'End keeper (1):1','End keeper (1):1',#9323,#9329,'End keeper (1):1');
#271=NEXT_ASSEMBLY_USAGE_OCCURRENCE('Pilot ring:1','Pilot ring:1',
'Pilot ring:1',#9323,#9330,'Pilot ring:1');
#272=NEXT_ASSEMBLY_USAGE_OCCURRENCE('End collar:1','End collar:1',
'End collar:1',#9323,#9331,'End collar:1');
#273=NEXT_ASSEMBLY_USAGE_OCCURRENCE('End collar (1):1',
'End collar (1):1','End collar (1):1',#9323,#9332,'End collar (1):1');
#274=NEXT_ASSEMBLY_USAGE_OCCURRENCE('Key 6x6x20:2','Key 6x6x20:2',
'Key 6x6x20:2',#9323,#9333,'Key 6x6x20:2');
#275=NEXT_ASSEMBLY_USAGE_OCCURRENCE('Socket Set Screw - M5x8:2',
'Socket Set Screw - M5x8:2','Socket Set Screw - M5x8:2',#9323,#9338,
'Socket Set Screw - M5x8:2');
#276=NEXT_ASSEMBLY_USAGE_OCCURRENCE('Cap Screw - M5x20:2',
'Cap Screw - M5x20:2','Cap Screw - M5x20:2',#9323,#9334,
'Cap Screw - M5x20:2');
#277=NEXT_ASSEMBLY_USAGE_OCCURRENCE('Key 6x6x20:3','Key 6x6x20:3',
'Key 6x6x20:3',#9323,#9333,'Key 6x6x20:3');
#278=NEXT_ASSEMBLY_USAGE_OCCURRENCE('Socket Set Screw - M5x8:3',
'Socket Set Screw - M5x8:3','Socket Set Screw - M5x8:3',#9323,#9338,
'Socket Set Screw - M5x8:3');
#279=NEXT_ASSEMBLY_USAGE_OCCURRENCE('Cap Screw - M5x20:3',
'Cap Screw - M5x20:3','Cap Screw - M5x20:3',#9323,#9334,
'Cap Screw - M5x20:3');
#280=NEXT_ASSEMBLY_USAGE_OCCURRENCE('Flat Washer - M6:6',
'Flat Washer - M6:6','Flat Washer - M6:6',#9323,#9336,
'Flat Washer - M6:6');
#281=NEXT_ASSEMBLY_USAGE_OCCURRENCE('Cap Screw - M6x25:6',
'Cap Screw - M6x25:6','Cap Screw - M6x25:6',#9323,#9335,
'Cap Screw - M6x25:6');
#282=NEXT_ASSEMBLY_USAGE_OCCURRENCE('Flat Washer - M6:7',
'Flat Washer - M6:7','Flat Washer - M6:7',#9323,#9336,
'Flat Washer - M6:7');
#283=NEXT_ASSEMBLY_USAGE_OCCURRENCE('Hex Nut - M6:2','Hex Nut - M6:2',
'Hex Nut - M6:2',#9323,#9337,'Hex Nut - M6:2');
#284=NEXT_ASSEMBLY_USAGE_OCCURRENCE('Flat Washer - M6:8',
'Flat Washer - M6:8','Flat Washer - M6:8',#9323,#9336,
'Flat Washer - M6:8');
#285=NEXT_ASSEMBLY_USAGE_OCCURRENCE('Cap Screw - M6x25:7',
'Cap Screw - M6x25:7','Cap Screw - M6x25:7',#9323,#9335,
'Cap Screw - M6x25:7');
#286=NEXT_ASSEMBLY_USAGE_OCCURRENCE('Flat Washer - M6:9',
'Flat Washer - M6:9','Flat Washer - M6:9',#9323,#9336,
'Flat Washer - M6:9');
#287=NEXT_ASSEMBLY_USAGE_OCCURRENCE('Hex Nut - M6:3','Hex Nut - M6:3',
'Hex Nut - M6:3',#9323,#9337,'Hex Nut - M6:3');
#288=NEXT_ASSEMBLY_USAGE_OCCURRENCE('Flat Washer - M6:10',
'Flat Washer - M6:10','Flat Washer - M6:10',#9323,#9336,
'Flat Washer - M6:10');
#289=NEXT_ASSEMBLY_USAGE_OCCURRENCE('Cap Screw - M6x25:8',
'Cap Screw - M6x25:8','Cap Screw - M6x25:8',#9323,#9335,
'Cap Screw - M6x25:8');
#290=NEXT_ASSEMBLY_USAGE_OCCURRENCE('Flat Washer - M6:11',
'Flat Washer - M6:11','Flat Washer - M6:11',#9323,#9336,
'Flat Washer - M6:11');
#291=NEXT_ASSEMBLY_USAGE_OCCURRENCE('Hex Nut - M6:4','Hex Nut - M6:4',
'Hex Nut - M6:4',#9323,#9337,'Hex Nut - M6:4');
#292=NEXT_ASSEMBLY_USAGE_OCCURRENCE('Flat Washer - M6:12',
'Flat Washer - M6:12','Flat Washer - M6:12',#9323,#9336,
'Flat Washer - M6:12');
#293=NEXT_ASSEMBLY_USAGE_OCCURRENCE('Cap Screw - M6x25:9',
'Cap Screw - M6x25:9','Cap Screw - M6x25:9',#9323,#9335,
'Cap Screw - M6x25:9');
#294=NEXT_ASSEMBLY_USAGE_OCCURRENCE('Flat Washer - M6:13',
'Flat Washer - M6:13','Flat Washer - M6:13',#9323,#9336,
'Flat Washer - M6:13');
#295=NEXT_ASSEMBLY_USAGE_OCCURRENCE('Hex Nut - M6:5','Hex Nut - M6:5',
'Hex Nut - M6:5',#9323,#9337,'Hex Nut - M6:5');
#296=NEXT_ASSEMBLY_USAGE_OCCURRENCE('Socket Set Screw - M5x8:4',
'Socket Set Screw - M5x8:4','Socket Set Screw - M5x8:4',#9323,#9338,
'Socket Set Screw - M5x8:4');
#297=NEXT_ASSEMBLY_USAGE_OCCURRENCE('Socket Set Screw - M5x8:5',
'Socket Set Screw - M5x8:5','Socket Set Screw - M5x8:5',#9323,#9338,
'Socket Set Screw - M5x8:5');
#298=NEXT_ASSEMBLY_USAGE_OCCURRENCE('Support frame:1','Support frame:1',
'Support frame:1',#9307,#9308,'Support frame:1');
#299=NEXT_ASSEMBLY_USAGE_OCCURRENCE('Coupled shafts:1',
'Coupled shafts:1','Coupled shafts:1',#9307,#9323,'Coupled shafts:1');
#300=B_SPLINE_CURVE_WITH_KNOTS('',3,(#7504,#7505,#7506,#7507,#7508,#7509,
#7510,#7511,#7512,#7513),.UNSPECIFIED.,.F.,.F.,(4,2,2,2,4),(1.13193471301885,
1.22626174930539,1.32058878559194,1.41491753480854,1.50924628402513),
 .UNSPECIFIED.);
#301=B_SPLINE_CURVE_WITH_KNOTS('',3,(#7515,#7516,#7517,#7518,#7519,#7520,
#7521,#7522,#7523,#7524,#7525,#7526,#7527,#7528,#7529,#7530,#7531,#7532),
 .UNSPECIFIED.,.F.,.F.,(4,2,2,2,2,2,2,2,4),(0.377311571006283,0.471638607292829,
0.565965643579376,0.66029439279597,0.754623142012565,0.84895189122916,0.943280640445754,
1.0376076767323,1.13193471301885),.UNSPECIFIED.);
#302=B_SPLINE_CURVE_WITH_KNOTS('',3,(#7533,#7534,#7535,#7536,#7537,#7538,
#7539,#7540,#7541,#7542),.UNSPECIFIED.,.F.,.F.,(4,2,2,2,4),(1.50924628402513,
1.60357503324173,1.69790378245832,1.79223081874487,1.88655785503141),
 .UNSPECIFIED.);
#303=B_SPLINE_CURVE_WITH_KNOTS('',3,(#7545,#7546,#7547,#7548,#7549,#7550,
#7551,#7552,#7553,#7554,#7555,#7556,#7557,#7558,#7559,#7560,#7561,#7562,
#7563,#7564,#7565,#7566,#7567,#7568,#7569,#7570,#7571,#7572,#7573,#7574,
#7575,#7576,#7577,#7578),.UNSPECIFIED.,.T.,.F.,(4,2,2,2,2,2,2,2,2,2,2,2,
2,2,2,2,4),(0.,0.0946120580087934,0.189224116017587,0.283822945575014,0.378421775132442,
0.47302060468987,0.567619434247297,0.662231492256091,0.756843550264884,
0.851455608273677,0.94606766628247,1.0406664958399,1.13526532539733,1.22986415495475,
1.32446298451218,1.41907504252097,1.51368710052977),.UNSPECIFIED.);
#304=B_SPLINE_CURVE_WITH_KNOTS('',3,(#7581,#7582,#7583,#7584,#7585,#7586,
#7587,#7588,#7589,#7590,#7591,#7592,#7593,#7594,#7595,#7596,#7597,#7598,
#7599,#7600,#7601,#7602,#7603,#7604,#7605,#7606,#7607,#7608,#7609,#7610,
#7611,#7612,#7613,#7614),.UNSPECIFIED.,.T.,.F.,(4,2,2,2,2,2,2,2,2,2,2,2,
2,2,2,2,4),(0.,0.0946120580087934,0.189224116017587,0.283822945575014,0.378421775132442,
0.47302060468987,0.567619434247297,0.66223149225609,0.756843550264884,0.851455608273677,
0.94606766628247,1.0406664958399,1.13526532539733,1.22986415495475,1.32446298451218,
1.41907504252097,1.51368710052977),.UNSPECIFIED.);
#305=B_SPLINE_CURVE_WITH_KNOTS('',3,(#7618,#7619,#7620,#7621,#7622,#7623,
#7624,#7625,#7626,#7627),.UNSPECIFIED.,.F.,.F.,(4,2,2,2,4),(1.13193471301885,
1.22626174930539,1.32058878559194,1.41491753480854,1.50924628402513),
 .UNSPECIFIED.);
#306=B_SPLINE_CURVE_WITH_KNOTS('',3,(#7629,#7630,#7631,#7632,#7633,#7634,
#7635,#7636,#7637,#7638,#7639,#7640,#7641,#7642,#7643,#7644,#7645,#7646),
 .UNSPECIFIED.,.F.,.F.,(4,2,2,2,2,2,2,2,4),(0.377311571006283,0.47163860729283,
0.565965643579376,0.660294392795971,0.754623142012565,0.84895189122916,
0.943280640445755,1.0376076767323,1.13193471301885),.UNSPECIFIED.);
#307=B_SPLINE_CURVE_WITH_KNOTS('',3,(#7647,#7648,#7649,#7650,#7651,#7652,
#7653,#7654,#7655,#7656),.UNSPECIFIED.,.F.,.F.,(4,2,2,2,4),(1.50924628402513,
1.60357503324173,1.69790378245832,1.79223081874487,1.88655785503141),
 .UNSPECIFIED.);
#308=B_SPLINE_CURVE_WITH_KNOTS('',3,(#7665,#7666,#7667,#7668,#7669,#7670,
#7671,#7672,#7673,#7674,#7675,#7676,#7677,#7678,#7679,#7680,#7681,#7682),
 .UNSPECIFIED.,.F.,.F.,(4,2,2,2,2,2,2,2,4),(0.377311571006282,0.471638607292829,
0.565965643579376,0.660294392795971,0.754623142012565,0.84895189122916,
0.943280640445754,1.0376076767323,1.13193471301885),.UNSPECIFIED.);
#309=B_SPLINE_CURVE_WITH_KNOTS('',3,(#7684,#7685,#7686,#7687,#7688,#7689,
#7690,#7691,#7692,#7693),.UNSPECIFIED.,.F.,.F.,(4,2,2,2,4),(1.13193471301885,
1.22626174930539,1.32058878559194,1.41491753480854,1.50924628402513),
 .UNSPECIFIED.);
#310=B_SPLINE_CURVE_WITH_KNOTS('',3,(#7694,#7695,#7696,#7697,#7698,#7699,
#7700,#7701,#7702,#7703),.UNSPECIFIED.,.F.,.F.,(4,2,2,2,4),(1.50924628402513,
1.60357503324172,1.69790378245832,1.79223081874487,1.88655785503141),
 .UNSPECIFIED.);
#311=B_SPLINE_CURVE_WITH_KNOTS('',3,(#7706,#7707,#7708,#7709,#7710,#7711,
#7712,#7713,#7714,#7715,#7716,#7717,#7718,#7719,#7720,#7721,#7722,#7723),
 .UNSPECIFIED.,.F.,.F.,(4,2,2,2,2,2,2,2,4),(0.377311571006283,0.47163860729283,
0.565965643579376,0.660294392795971,0.754623142012565,0.84895189122916,
0.943280640445754,1.0376076767323,1.13193471301885),.UNSPECIFIED.);
#312=B_SPLINE_CURVE_WITH_KNOTS('',3,(#7725,#7726,#7727,#7728,#7729,#7730,
#7731,#7732,#7733,#7734),.UNSPECIFIED.,.F.,.F.,(4,2,2,2,4),(1.13193471301885,
1.22626174930539,1.32058878559194,1.41491753480854,1.50924628402513),
 .UNSPECIFIED.);
#313=B_SPLINE_CURVE_WITH_KNOTS('',3,(#7735,#7736,#7737,#7738,#7739,#7740,
#7741,#7742,#7743,#7744),.UNSPECIFIED.,.F.,.F.,(4,2,2,2,4),(1.50924628402513,
1.60357503324173,1.69790378245832,1.79223081874487,1.88655785503141),
 .UNSPECIFIED.);
#314=B_SPLINE_CURVE_WITH_KNOTS('',3,(#7747,#7748,#7749,#7750,#7751,#7752,
#7753,#7754,#7755,#7756,#7757,#7758,#7759,#7760,#7761,#7762,#7763,#7764),
 .UNSPECIFIED.,.F.,.F.,(4,2,2,2,2,2,2,2,4),(0.377311571006282,0.471638607292829,
0.565965643579376,0.66029439279597,0.754623142012565,0.84895189122916,0.943280640445754,
1.0376076767323,1.13193471301885),.UNSPECIFIED.);
#315=B_SPLINE_CURVE_WITH_KNOTS('',3,(#7766,#7767,#7768,#7769,#7770,#7771,
#7772,#7773,#7774,#7775),.UNSPECIFIED.,.F.,.F.,(4,2,2,2,4),(1.13193471301885,
1.22626174930539,1.32058878559194,1.41491753480854,1.50924628402513),
 .UNSPECIFIED.);
#316=B_SPLINE_CURVE_WITH_KNOTS('',3,(#7776,#7777,#7778,#7779,#7780,#7781,
#7782,#7783,#7784,#7785),.UNSPECIFIED.,.F.,.F.,(4,2,2,2,4),(1.50924628402513,
1.60357503324172,1.69790378245832,1.79223081874487,1.88655785503141),
 .UNSPECIFIED.);
#317=B_SPLINE_CURVE_WITH_KNOTS('',3,(#7788,#7789,#7790,#7791,#7792,#7793,
#7794,#7795,#7796,#7797,#7798,#7799,#7800,#7801,#7802,#7803,#7804,#7805),
 .UNSPECIFIED.,.F.,.F.,(4,2,2,2,2,2,2,2,4),(0.377311571006283,0.471638607292829,
0.565965643579376,0.660294392795971,0.754623142012565,0.84895189122916,
0.943280640445755,1.0376076767323,1.13193471301885),.UNSPECIFIED.);
#318=B_SPLINE_CURVE_WITH_KNOTS('',3,(#7807,#7808,#7809,#7810,#7811,#7812,
#7813,#7814,#7815,#7816),.UNSPECIFIED.,.F.,.F.,(4,2,2,2,4),(1.13193471301885,
1.22626174930539,1.32058878559194,1.41491753480854,1.50924628402513),
 .UNSPECIFIED.);
#319=B_SPLINE_CURVE_WITH_KNOTS('',3,(#7817,#7818,#7819,#7820,#7821,#7822,
#7823,#7824,#7825,#7826),.UNSPECIFIED.,.F.,.F.,(4,2,2,2,4),(1.50924628402513,
1.60357503324172,1.69790378245832,1.79223081874487,1.88655785503141),
 .UNSPECIFIED.);
#320=B_SPLINE_CURVE_WITH_KNOTS('',3,(#7830,#7831,#7832,#7833,#7834,#7835,
#7836,#7837,#7838,#7839,#7840,#7841,#7842,#7843,#7844,#7845,#7846,#7847,
#7848,#7849,#7850,#7851,#7852,#7853,#7854,#7855,#7856,#7857,#7858,#7859,
#7860,#7861,#7862,#7863),.UNSPECIFIED.,.T.,.F.,(4,2,2,2,2,2,2,2,2,2,2,2,
2,2,2,2,4),(0.,0.0946120580087934,0.189224116017587,0.283822945575014,0.378421775132442,
0.47302060468987,0.567619434247297,0.66223149225609,0.756843550264884,0.851455608273677,
0.94606766628247,1.0406664958399,1.13526532539733,1.22986415495475,1.32446298451218,
1.41907504252097,1.51368710052977),.UNSPECIFIED.);
#321=B_SPLINE_CURVE_WITH_KNOTS('',3,(#7866,#7867,#7868,#7869,#7870,#7871,
#7872,#7873,#7874,#7875,#7876,#7877,#7878,#7879,#7880,#7881,#7882,#7883,
#7884,#7885,#7886,#7887,#7888,#7889,#7890,#7891,#7892,#7893,#7894,#7895,
#7896,#7897,#7898,#7899),.UNSPECIFIED.,.T.,.F.,(4,2,2,2,2,2,2,2,2,2,2,2,
2,2,2,2,4),(0.,0.0946120580087934,0.189224116017587,0.283822945575014,0.378421775132442,
0.47302060468987,0.567619434247297,0.66223149225609,0.756843550264884,0.851455608273677,
0.94606766628247,1.0406664958399,1.13526532539733,1.22986415495475,1.32446298451218,
1.41907504252097,1.51368710052977),.UNSPECIFIED.);
#322=B_SPLINE_CURVE_WITH_KNOTS('',3,(#7904,#7905,#7906,#7907,#7908,#7909,
#7910,#7911,#7912,#7913,#7914,#7915,#7916,#7917,#7918,#7919,#7920,#7921,
#7922,#7923,#7924,#7925,#7926,#7927,#7928,#7929,#7930,#7931,#7932,#7933,
#7934,#7935,#7936,#7937),.UNSPECIFIED.,.T.,.F.,(4,2,2,2,2,2,2,2,2,2,2,2,
2,2,2,2,4),(0.,0.0946120580087934,0.189224116017587,0.283822945575014,0.378421775132442,
0.47302060468987,0.567619434247297,0.66223149225609,0.756843550264884,0.851455608273677,
0.94606766628247,1.0406664958399,1.13526532539733,1.22986415495475,1.32446298451218,
1.41907504252097,1.51368710052977),.UNSPECIFIED.);
#323=B_SPLINE_CURVE_WITH_KNOTS('',3,(#7940,#7941,#7942,#7943,#7944,#7945,
#7946,#7947,#7948,#7949,#7950,#7951,#7952,#7953,#7954,#7955,#7956,#7957,
#7958,#7959,#7960,#7961,#7962,#7963,#7964,#7965,#7966,#7967,#7968,#7969,
#7970,#7971,#7972,#7973),.UNSPECIFIED.,.T.,.F.,(4,2,2,2,2,2,2,2,2,2,2,2,
2,2,2,2,4),(0.,0.0946120580087934,0.189224116017587,0.283822945575014,0.378421775132442,
0.47302060468987,0.567619434247297,0.66223149225609,0.756843550264884,0.851455608273677,
0.94606766628247,1.0406664958399,1.13526532539733,1.22986415495475,1.32446298451218,
1.41907504252097,1.51368710052977),.UNSPECIFIED.);
#324=B_SPLINE_CURVE_WITH_KNOTS('',3,(#8147,#8148,#8149,#8150,#8151,#8152,
#8153,#8154,#8155,#8156),.UNSPECIFIED.,.F.,.F.,(4,2,2,2,4),(0.803821788694083,
0.87295099185362,0.95230721290097,1.03166343394832,1.10079263710786),
 .UNSPECIFIED.);
#325=B_SPLINE_CURVE_WITH_KNOTS('',3,(#8162,#8163,#8164,#8165,#8166,#8167,
#8168,#8169,#8170,#8171,#8172,#8173,#8174,#8175,#8176,#8177,#8178,#8179),
 .UNSPECIFIED.,.F.,.F.,(4,2,2,2,2,2,2,2,4),(0.,0.0791914196064458,0.158382839212892,
0.237573628052636,0.31676441689238,0.395955205732124,0.475145994571868,
0.554337414178314,0.63352883378476),.UNSPECIFIED.);
#326=B_SPLINE_CURVE_WITH_KNOTS('',3,(#8180,#8181,#8182,#8183,#8184,#8185,
#8186,#8187,#8188,#8189,#8190,#8191,#8192,#8193,#8194,#8195,#8196,#8197),
 .UNSPECIFIED.,.F.,.F.,(4,2,2,2,2,2,2,2,4),(0.63352883378476,0.712720253391205,
0.791911672997651,0.871102461837395,0.95029325067714,1.02948403951688,1.10867482835663,
1.18786624796307,1.26705766756952),.UNSPECIFIED.);
#327=B_SPLINE_CURVE_WITH_KNOTS('',3,(#8200,#8201,#8202,#8203,#8204,#8205,
#8206,#8207,#8208,#8209),.UNSPECIFIED.,.F.,.F.,(4,2,2,2,4),(0.168950313426771,
0.238079516586307,0.317435737633657,0.396791958681006,0.465921161840542),
 .UNSPECIFIED.);
#328=B_SPLINE_CURVE_WITH_KNOTS('',3,(#8346,#8347,#8348,#8349,#8350,#8351,
#8352,#8353,#8354,#8355),.UNSPECIFIED.,.F.,.F.,(4,2,2,2,4),(0.803821788694084,
0.87295099185362,0.95230721290097,1.03166343394832,1.10079263710786),
 .UNSPECIFIED.);
#329=B_SPLINE_CURVE_WITH_KNOTS('',3,(#8361,#8362,#8363,#8364,#8365,#8366,
#8367,#8368,#8369,#8370,#8371,#8372,#8373,#8374,#8375,#8376,#8377,#8378),
 .UNSPECIFIED.,.F.,.F.,(4,2,2,2,2,2,2,2,4),(0.,0.0791914196064459,0.158382839212892,
0.237573628052636,0.31676441689238,0.395955205732124,0.475145994571868,
0.554337414178314,0.63352883378476),.UNSPECIFIED.);
#330=B_SPLINE_CURVE_WITH_KNOTS('',3,(#8379,#8380,#8381,#8382,#8383,#8384,
#8385,#8386,#8387,#8388,#8389,#8390,#8391,#8392,#8393,#8394,#8395,#8396),
 .UNSPECIFIED.,.F.,.F.,(4,2,2,2,2,2,2,2,4),(0.63352883378476,0.712720253391206,
0.791911672997652,0.871102461837396,0.95029325067714,1.02948403951688,1.10867482835663,
1.18786624796307,1.26705766756952),.UNSPECIFIED.);
#331=B_SPLINE_CURVE_WITH_KNOTS('',3,(#8399,#8400,#8401,#8402,#8403,#8404,
#8405,#8406,#8407,#8408),.UNSPECIFIED.,.F.,.F.,(4,2,2,2,4),(0.168950313426773,
0.238079516586307,0.317435737633657,0.396791958681006,0.465921161840543),
 .UNSPECIFIED.);
#332=B_SPLINE_CURVE_WITH_KNOTS('',3,(#8495,#8496,#8497,#8498,#8499,#8500,
#8501,#8502,#8503,#8504,#8505,#8506,#8507,#8508),.UNSPECIFIED.,.F.,.F.,
(4,2,2,2,2,2,4),(0.75600573798702,0.793568827564647,0.872922520054201,0.952276212543756,
1.03162990503331,1.11098359752287,1.14854668710049),.UNSPECIFIED.);
#333=B_SPLINE_CURVE_WITH_KNOTS('',3,(#8514,#8515,#8516,#8517,#8518,#8519,
#8520,#8521,#8522,#8523,#8524,#8525,#8526,#8527,#8528,#8529,#8530,#8531),
 .UNSPECIFIED.,.F.,.F.,(4,2,2,2,2,2,2,2,4),(0.,0.079216580773363,0.158433161546726,
0.23764869707457,0.316864232602414,0.396079768130259,0.475295303658103,
0.554511884431466,0.633728465204829),.UNSPECIFIED.);
#334=B_SPLINE_CURVE_WITH_KNOTS('',3,(#8532,#8533,#8534,#8535,#8536,#8537,
#8538,#8539,#8540,#8541,#8542,#8543,#8544,#8545,#8546,#8547,#8548,#8549),
 .UNSPECIFIED.,.F.,.F.,(4,2,2,2,2,2,2,2,4),(0.633728465204829,0.712945045978192,
0.792161626751555,0.871377162279399,0.950592697807243,1.02980823333509,
1.10902376886293,1.18824034963629,1.26745693040966),.UNSPECIFIED.);
#335=B_SPLINE_CURVE_WITH_KNOTS('',3,(#8552,#8553,#8554,#8555,#8556,#8557,
#8558,#8559,#8560,#8561,#8562,#8563,#8564,#8565),.UNSPECIFIED.,.F.,.F.,
(4,2,2,2,2,2,4),(0.121154929624515,0.158718019202143,0.238071711691697,
0.317425404181252,0.396779096670807,0.476132789160362,0.513695878737989),
 .UNSPECIFIED.);
#336=B_SPLINE_CURVE_WITH_KNOTS('',3,(#8590,#8591,#8592,#8593,#8594,#8595,
#8596,#8597,#8598,#8599,#8600,#8601,#8602,#8603),.UNSPECIFIED.,.F.,.F.,
(4,2,2,2,2,2,4),(0.756005737987019,0.793568827564645,0.8729225200542,0.952276212543755,
1.03162990503331,1.11098359752287,1.14854668710049),.UNSPECIFIED.);
#337=B_SPLINE_CURVE_WITH_KNOTS('',3,(#8609,#8610,#8611,#8612,#8613,#8614,
#8615,#8616,#8617,#8618,#8619,#8620,#8621,#8622,#8623,#8624,#8625,#8626),
 .UNSPECIFIED.,.F.,.F.,(4,2,2,2,2,2,2,2,4),(0.,0.0792165807733624,0.158433161546725,
0.23764869707457,0.316864232602414,0.396079768130259,0.475295303658103,
0.554511884431466,0.633728465204828),.UNSPECIFIED.);
#338=B_SPLINE_CURVE_WITH_KNOTS('',3,(#8627,#8628,#8629,#8630,#8631,#8632,
#8633,#8634,#8635,#8636,#8637,#8638,#8639,#8640,#8641,#8642,#8643,#8644),
 .UNSPECIFIED.,.F.,.F.,(4,2,2,2,2,2,2,2,4),(0.633728465204828,0.712945045978191,
0.792161626751553,0.871377162279398,0.950592697807242,1.02980823333509,
1.10902376886293,1.18824034963629,1.26745693040966),.UNSPECIFIED.);
#339=B_SPLINE_CURVE_WITH_KNOTS('',3,(#8647,#8648,#8649,#8650,#8651,#8652,
#8653,#8654,#8655,#8656,#8657,#8658,#8659,#8660),.UNSPECIFIED.,.F.,.F.,
(4,2,2,2,2,2,4),(0.121154929624521,0.158718019202141,0.238071711691696,
0.317425404181252,0.396779096670807,0.476132789160362,0.513695878737985),
 .UNSPECIFIED.);
#340=SPHERICAL_SURFACE('',#5210,2.35);
#341=SPHERICAL_SURFACE('',#5250,2.35);
#342=SHAPE_REPRESENTATION_RELATIONSHIP('SRR','None',#9276,#370);
#343=SHAPE_REPRESENTATION_RELATIONSHIP('SRR','None',#9277,#371);
#344=SHAPE_REPRESENTATION_RELATIONSHIP('SRR','None',#9278,#372);
#345=SHAPE_REPRESENTATION_RELATIONSHIP('SRR','None',#9279,#373);
#346=SHAPE_REPRESENTATION_RELATIONSHIP('SRR','None',#9280,#374);
#347=SHAPE_REPRESENTATION_RELATIONSHIP('SRR','None',#9281,#375);
#348=SHAPE_REPRESENTATION_RELATIONSHIP('SRR','None',#9282,#376);
#349=SHAPE_REPRESENTATION_RELATIONSHIP('SRR','None',#9283,#377);
#350=SHAPE_REPRESENTATION_RELATIONSHIP('SRR','None',#9284,#378);
#351=SHAPE_REPRESENTATION_RELATIONSHIP('SRR','None',#9286,#379);
#352=SHAPE_REPRESENTATION_RELATIONSHIP('SRR','None',#9287,#380);
#353=SHAPE_REPRESENTATION_RELATIONSHIP('SRR','None',#9288,#381);
#354=SHAPE_REPRESENTATION_RELATIONSHIP('SRR','None',#9289,#382);
#355=SHAPE_REPRESENTATION_RELATIONSHIP('SRR','None',#9291,#383);
#356=SHAPE_REPRESENTATION_RELATIONSHIP('SRR','None',#9292,#384);
#357=SHAPE_REPRESENTATION_RELATIONSHIP('SRR','None',#9293,#385);
#358=SHAPE_REPRESENTATION_RELATIONSHIP('SRR','None',#9294,#386);
#359=SHAPE_REPRESENTATION_RELATIONSHIP('SRR','None',#9295,#387);
#360=SHAPE_REPRESENTATION_RELATIONSHIP('SRR','None',#9296,#388);
#361=SHAPE_REPRESENTATION_RELATIONSHIP('SRR','None',#9297,#389);
#362=SHAPE_REPRESENTATION_RELATIONSHIP('SRR','None',#9298,#390);
#363=SHAPE_REPRESENTATION_RELATIONSHIP('SRR','None',#9299,#391);
#364=SHAPE_REPRESENTATION_RELATIONSHIP('SRR','None',#9300,#392);
#365=SHAPE_REPRESENTATION_RELATIONSHIP('SRR','None',#9301,#393);
#366=SHAPE_REPRESENTATION_RELATIONSHIP('SRR','None',#9302,#394);
#367=SHAPE_REPRESENTATION_RELATIONSHIP('SRR','None',#9303,#395);
#368=SHAPE_REPRESENTATION_RELATIONSHIP('SRR','None',#9304,#396);
#369=SHAPE_REPRESENTATION_RELATIONSHIP('SRR','None',#9305,#397);
#370=ADVANCED_BREP_SHAPE_REPRESENTATION('',(#427),#9111);
#371=ADVANCED_BREP_SHAPE_REPRESENTATION('',(#428),#9112);
#372=ADVANCED_BREP_SHAPE_REPRESENTATION('',(#429),#9113);
#373=ADVANCED_BREP_SHAPE_REPRESENTATION('',(#430),#9114);
#374=ADVANCED_BREP_SHAPE_REPRESENTATION('',(#431),#9115);
#375=ADVANCED_BREP_SHAPE_REPRESENTATION('',(#432),#9116);
#376=ADVANCED_BREP_SHAPE_REPRESENTATION('',(#433),#9117);
#377=ADVANCED_BREP_SHAPE_REPRESENTATION('',(#434),#9118);
#378=ADVANCED_BREP_SHAPE_REPRESENTATION('',(#435),#9119);
#379=ADVANCED_BREP_SHAPE_REPRESENTATION('',(#436),#9121);
#380=ADVANCED_BREP_SHAPE_REPRESENTATION('',(#437,#438),#9122);
#381=ADVANCED_BREP_SHAPE_REPRESENTATION('',(#439),#9123);
#382=ADVANCED_BREP_SHAPE_REPRESENTATION('',(#41),#9124);
#383=ADVANCED_BREP_SHAPE_REPRESENTATION('',(#440),#9126);
#384=ADVANCED_BREP_SHAPE_REPRESENTATION('',(#441),#9127);
#385=ADVANCED_BREP_SHAPE_REPRESENTATION('',(#442),#9128);
#386=ADVANCED_BREP_SHAPE_REPRESENTATION('',(#443),#9129);
#387=ADVANCED_BREP_SHAPE_REPRESENTATION('',(#444),#9130);
#388=ADVANCED_BREP_SHAPE_REPRESENTATION('',(#445),#9131);
#389=ADVANCED_BREP_SHAPE_REPRESENTATION('',(#446),#9132);
#390=ADVANCED_BREP_SHAPE_REPRESENTATION('',(#447),#9133);
#391=ADVANCED_BREP_SHAPE_REPRESENTATION('',(#448),#9134);
#392=ADVANCED_BREP_SHAPE_REPRESENTATION('',(#449),#9135);
#393=ADVANCED_BREP_SHAPE_REPRESENTATION('',(#42),#9136);
#394=ADVANCED_BREP_SHAPE_REPRESENTATION('',(#43),#9137);
#395=ADVANCED_BREP_SHAPE_REPRESENTATION('',(#450),#9138);
#396=ADVANCED_BREP_SHAPE_REPRESENTATION('',(#451),#9139);
#397=ADVANCED_BREP_SHAPE_REPRESENTATION('',(#452),#9140);
#398=STYLED_ITEM('',(#9479),#427);
#399=STYLED_ITEM('',(#9514),#428);
#400=STYLED_ITEM('',(#9514),#429);
#401=STYLED_ITEM('',(#9500),#430);
#402=STYLED_ITEM('',(#9493),#431);
#403=STYLED_ITEM('',(#9493),#432);
#404=STYLED_ITEM('',(#9500),#433);
#405=STYLED_ITEM('',(#9493),#434);
#406=STYLED_ITEM('',(#9493),#435);
#407=STYLED_ITEM('',(#9479),#436);
#408=STYLED_ITEM('',(#9500),#437);
#409=STYLED_ITEM('',(#9500),#438);
#410=STYLED_ITEM('',(#9507),#439);
#411=STYLED_ITEM('',(#9507),#41);
#412=STYLED_ITEM('',(#9500),#440);
#413=STYLED_ITEM('',(#9493),#441);
#414=STYLED_ITEM('',(#9514),#442);
#415=STYLED_ITEM('',(#9500),#443);
#416=STYLED_ITEM('',(#9486),#444);
#417=STYLED_ITEM('',(#9514),#445);
#418=STYLED_ITEM('',(#9493),#446);
#419=STYLED_ITEM('',(#9486),#447);
#420=STYLED_ITEM('',(#9486),#448);
#421=STYLED_ITEM('',(#9500),#449);
#422=STYLED_ITEM('',(#9507),#42);
#423=STYLED_ITEM('',(#9507),#43);
#424=STYLED_ITEM('',(#9507),#450);
#425=STYLED_ITEM('',(#9507),#451);
#426=STYLED_ITEM('',(#9507),#452);
#427=MANIFOLD_SOLID_BREP('Body1',#4752);
#428=MANIFOLD_SOLID_BREP('Body1',#4753);
#429=MANIFOLD_SOLID_BREP('Body1',#4754);
#430=MANIFOLD_SOLID_BREP('Body1',#4755);
#431=MANIFOLD_SOLID_BREP('Body1',#4756);
#432=MANIFOLD_SOLID_BREP('Body1',#4757);
#433=MANIFOLD_SOLID_BREP('Body1',#4758);
#434=MANIFOLD_SOLID_BREP('Body1',#4759);
#435=MANIFOLD_SOLID_BREP('Body1',#4760);
#436=MANIFOLD_SOLID_BREP('Body1',#4761);
#437=MANIFOLD_SOLID_BREP('Body1',#4762);
#438=MANIFOLD_SOLID_BREP('Body2',#4763);
#439=MANIFOLD_SOLID_BREP('Body1',#4764);
#440=MANIFOLD_SOLID_BREP('Body1',#4767);
#441=MANIFOLD_SOLID_BREP('Body1',#4768);
#442=MANIFOLD_SOLID_BREP('Body1',#4769);
#443=MANIFOLD_SOLID_BREP('Body1',#4770);
#444=MANIFOLD_SOLID_BREP('Body1',#4771);
#445=MANIFOLD_SOLID_BREP('Body1',#4772);
#446=MANIFOLD_SOLID_BREP('Body1',#4773);
#447=MANIFOLD_SOLID_BREP('Body1',#4774);
#448=MANIFOLD_SOLID_BREP('Body1',#4775);
#449=MANIFOLD_SOLID_BREP('Body1',#4776);
#450=MANIFOLD_SOLID_BREP('Body1',#4781);
#451=MANIFOLD_SOLID_BREP('Body1',#4782);
#452=MANIFOLD_SOLID_BREP('Body1',#4783);
#453=FACE_BOUND('',#1025,.T.);
#454=FACE_BOUND('',#1026,.T.);
#455=FACE_BOUND('',#1027,.T.);
#456=FACE_BOUND('',#1028,.T.);
#457=FACE_BOUND('',#1030,.T.);
#458=FACE_BOUND('',#1031,.T.);
#459=FACE_BOUND('',#1032,.T.);
#460=FACE_BOUND('',#1033,.T.);
#461=FACE_BOUND('',#1055,.T.);
#462=FACE_BOUND('',#1056,.T.);
#463=FACE_BOUND('',#1057,.T.);
#464=FACE_BOUND('',#1058,.T.);
#465=FACE_BOUND('',#1060,.T.);
#466=FACE_BOUND('',#1061,.T.);
#467=FACE_BOUND('',#1062,.T.);
#468=FACE_BOUND('',#1063,.T.);
#469=FACE_BOUND('',#1067,.T.);
#470=FACE_BOUND('',#1069,.T.);
#471=FACE_BOUND('',#1073,.T.);
#472=FACE_BOUND('',#1075,.T.);
#473=FACE_BOUND('',#1085,.T.);
#474=FACE_BOUND('',#1086,.T.);
#475=FACE_BOUND('',#1087,.T.);
#476=FACE_BOUND('',#1088,.T.);
#477=FACE_BOUND('',#1090,.T.);
#478=FACE_BOUND('',#1091,.T.);
#479=FACE_BOUND('',#1092,.T.);
#480=FACE_BOUND('',#1093,.T.);
#481=FACE_BOUND('',#1097,.T.);
#482=FACE_BOUND('',#1099,.T.);
#483=FACE_BOUND('',#1103,.T.);
#484=FACE_BOUND('',#1105,.T.);
#485=FACE_BOUND('',#1109,.T.);
#486=FACE_BOUND('',#1110,.T.);
#487=FACE_BOUND('',#1118,.T.);
#488=FACE_BOUND('',#1119,.T.);
#489=FACE_BOUND('',#1120,.T.);
#490=FACE_BOUND('',#1123,.T.);
#491=FACE_BOUND('',#1125,.T.);
#492=FACE_BOUND('',#1138,.T.);
#493=FACE_BOUND('',#1139,.T.);
#494=FACE_BOUND('',#1140,.T.);
#495=FACE_BOUND('',#1143,.T.);
#496=FACE_BOUND('',#1145,.T.);
#497=FACE_BOUND('',#1146,.T.);
#498=FACE_BOUND('',#1148,.T.);
#499=FACE_BOUND('',#1152,.T.);
#500=FACE_BOUND('',#1153,.T.);
#501=FACE_BOUND('',#1154,.T.);
#502=FACE_BOUND('',#1155,.T.);
#503=FACE_BOUND('',#1156,.T.);
#504=FACE_BOUND('',#1157,.T.);
#505=FACE_BOUND('',#1163,.T.);
#506=FACE_BOUND('',#1165,.T.);
#507=FACE_BOUND('',#1168,.T.);
#508=FACE_BOUND('',#1170,.T.);
#509=FACE_BOUND('',#1171,.T.);
#510=FACE_BOUND('',#1172,.T.);
#511=FACE_BOUND('',#1173,.T.);
#512=FACE_BOUND('',#1174,.T.);
#513=FACE_BOUND('',#1175,.T.);
#514=FACE_BOUND('',#1179,.T.);
#515=FACE_BOUND('',#1181,.T.);
#516=FACE_BOUND('',#1196,.T.);
#517=FACE_BOUND('',#1207,.T.);
#518=FACE_BOUND('',#1210,.T.);
#519=FACE_BOUND('',#1222,.T.);
#520=FACE_BOUND('',#1225,.T.);
#521=FACE_BOUND('',#1227,.T.);
#522=FACE_BOUND('',#1228,.T.);
#523=FACE_BOUND('',#1229,.T.);
#524=FACE_BOUND('',#1230,.T.);
#525=FACE_BOUND('',#1231,.T.);
#526=FACE_BOUND('',#1234,.T.);
#527=FACE_BOUND('',#1236,.T.);
#528=FACE_BOUND('',#1238,.T.);
#529=FACE_BOUND('',#1239,.T.);
#530=FACE_BOUND('',#1240,.T.);
#531=FACE_BOUND('',#1241,.T.);
#532=FACE_BOUND('',#1242,.T.);
#533=FACE_BOUND('',#1246,.T.);
#534=FACE_BOUND('',#1248,.T.);
#535=FACE_BOUND('',#1257,.T.);
#536=FACE_BOUND('',#1259,.T.);
#537=FACE_BOUND('',#1272,.T.);
#538=FACE_BOUND('',#1274,.T.);
#539=FACE_BOUND('',#1277,.T.);
#540=FACE_BOUND('',#1278,.T.);
#541=FACE_BOUND('',#1279,.T.);
#542=FACE_BOUND('',#1280,.T.);
#543=FACE_BOUND('',#1281,.T.);
#544=FACE_BOUND('',#1284,.T.);
#545=FACE_BOUND('',#1286,.T.);
#546=FACE_BOUND('',#1288,.T.);
#547=FACE_BOUND('',#1289,.T.);
#548=FACE_BOUND('',#1290,.T.);
#549=FACE_BOUND('',#1291,.T.);
#550=FACE_BOUND('',#1292,.T.);
#551=FACE_BOUND('',#1296,.T.);
#552=FACE_BOUND('',#1298,.T.);
#553=FACE_BOUND('',#1302,.T.);
#554=FACE_BOUND('',#1304,.T.);
#555=FACE_BOUND('',#1309,.T.);
#556=FACE_BOUND('',#1311,.T.);
#557=FACE_BOUND('',#1313,.T.);
#558=FACE_BOUND('',#1315,.T.);
#559=FACE_BOUND('',#1320,.T.);
#560=FACE_BOUND('',#1322,.T.);
#561=FACE_BOUND('',#1324,.T.);
#562=FACE_BOUND('',#1326,.T.);
#563=FACE_BOUND('',#1342,.T.);
#564=FACE_BOUND('',#1360,.T.);
#565=FACE_BOUND('',#1376,.T.);
#566=FACE_BOUND('',#1378,.T.);
#567=FACE_BOUND('',#1389,.T.);
#568=FACE_BOUND('',#1391,.T.);
#569=FACE_BOUND('',#1400,.T.);
#570=PLANE('',#5108);
#571=PLANE('',#5109);
#572=PLANE('',#5110);
#573=PLANE('',#5111);
#574=PLANE('',#5112);
#575=PLANE('',#5113);
#576=PLANE('',#5115);
#577=PLANE('',#5116);
#578=PLANE('',#5117);
#579=PLANE('',#5118);
#580=PLANE('',#5119);
#581=PLANE('',#5120);
#582=PLANE('',#5122);
#583=PLANE('',#5123);
#584=PLANE('',#5124);
#585=PLANE('',#5125);
#586=PLANE('',#5126);
#587=PLANE('',#5127);
#588=PLANE('',#5141);
#589=PLANE('',#5142);
#590=PLANE('',#5143);
#591=PLANE('',#5144);
#592=PLANE('',#5145);
#593=PLANE('',#5146);
#594=PLANE('',#5154);
#595=PLANE('',#5155);
#596=PLANE('',#5163);
#597=PLANE('',#5164);
#598=PLANE('',#5178);
#599=PLANE('',#5179);
#600=PLANE('',#5180);
#601=PLANE('',#5181);
#602=PLANE('',#5182);
#603=PLANE('',#5183);
#604=PLANE('',#5191);
#605=PLANE('',#5192);
#606=PLANE('',#5200);
#607=PLANE('',#5201);
#608=PLANE('',#5212);
#609=PLANE('',#5214);
#610=PLANE('',#5216);
#611=PLANE('',#5218);
#612=PLANE('',#5219);
#613=PLANE('',#5221);
#614=PLANE('',#5222);
#615=PLANE('',#5228);
#616=PLANE('',#5229);
#617=PLANE('',#5230);
#618=PLANE('',#5231);
#619=PLANE('',#5232);
#620=PLANE('',#5233);
#621=PLANE('',#5234);
#622=PLANE('',#5239);
#623=PLANE('',#5240);
#624=PLANE('',#5241);
#625=PLANE('',#5242);
#626=PLANE('',#5243);
#627=PLANE('',#5248);
#628=PLANE('',#5253);
#629=PLANE('',#5263);
#630=PLANE('',#5265);
#631=PLANE('',#5269);
#632=PLANE('',#5281);
#633=PLANE('',#5282);
#634=PLANE('',#5284);
#635=PLANE('',#5285);
#636=PLANE('',#5286);
#637=PLANE('',#5287);
#638=PLANE('',#5288);
#639=PLANE('',#5289);
#640=PLANE('',#5290);
#641=PLANE('',#5291);
#642=PLANE('',#5292);
#643=PLANE('',#5294);
#644=PLANE('',#5302);
#645=PLANE('',#5312);
#646=PLANE('',#5313);
#647=PLANE('',#5314);
#648=PLANE('',#5316);
#649=PLANE('',#5317);
#650=PLANE('',#5318);
#651=PLANE('',#5323);
#652=PLANE('',#5324);
#653=PLANE('',#5338);
#654=PLANE('',#5343);
#655=PLANE('',#5344);
#656=PLANE('',#5345);
#657=PLANE('',#5346);
#658=PLANE('',#5347);
#659=PLANE('',#5353);
#660=PLANE('',#5355);
#661=PLANE('',#5362);
#662=PLANE('',#5370);
#663=PLANE('',#5371);
#664=PLANE('',#5376);
#665=PLANE('',#5377);
#666=PLANE('',#5378);
#667=PLANE('',#5380);
#668=PLANE('',#5381);
#669=PLANE('',#5382);
#670=PLANE('',#5387);
#671=PLANE('',#5388);
#672=PLANE('',#5402);
#673=PLANE('',#5407);
#674=PLANE('',#5408);
#675=PLANE('',#5409);
#676=PLANE('',#5410);
#677=PLANE('',#5411);
#678=PLANE('',#5418);
#679=PLANE('',#5425);
#680=PLANE('',#5426);
#681=PLANE('',#5434);
#682=PLANE('',#5435);
#683=PLANE('',#5443);
#684=PLANE('',#5444);
#685=PLANE('',#5446);
#686=PLANE('',#5451);
#687=PLANE('',#5458);
#688=PLANE('',#5459);
#689=PLANE('',#5461);
#690=PLANE('',#5466);
#691=PLANE('',#5473);
#692=PLANE('',#5474);
#693=PLANE('',#5476);
#694=PLANE('',#5477);
#695=PLANE('',#5478);
#696=PLANE('',#5479);
#697=PLANE('',#5480);
#698=PLANE('',#5481);
#699=PLANE('',#5482);
#700=PLANE('',#5483);
#701=PLANE('',#5484);
#702=PLANE('',#5485);
#703=PLANE('',#5487);
#704=PLANE('',#5495);
#705=PLANE('',#5503);
#706=PLANE('',#5504);
#707=PLANE('',#5505);
#708=PLANE('',#5506);
#709=PLANE('',#5507);
#710=PLANE('',#5508);
#711=PLANE('',#5509);
#712=PLANE('',#5510);
#713=PLANE('',#5511);
#714=PLANE('',#5513);
#715=PLANE('',#5521);
#716=PLANE('',#5529);
#717=PLANE('',#5530);
#718=PLANE('',#5531);
#719=PLANE('',#5532);
#720=PLANE('',#5533);
#721=PLANE('',#5534);
#722=PLANE('',#5535);
#723=PLANE('',#5536);
#724=PLANE('',#5537);
#725=PLANE('',#5545);
#726=PLANE('',#5546);
#727=PLANE('',#5579);
#728=PLANE('',#5580);
#729=PLANE('',#5581);
#730=PLANE('',#5585);
#731=PLANE('',#5586);
#732=PLANE('',#5587);
#733=PLANE('',#5588);
#734=PLANE('',#5589);
#735=PLANE('',#5591);
#736=PLANE('',#5592);
#737=PLANE('',#5593);
#738=PLANE('',#5594);
#739=PLANE('',#5595);
#740=PLANE('',#5596);
#741=PLANE('',#5597);
#742=PLANE('',#5598);
#743=PLANE('',#5606);
#744=FACE_OUTER_BOUND('',#1016,.T.);
#745=FACE_OUTER_BOUND('',#1017,.T.);
#746=FACE_OUTER_BOUND('',#1018,.T.);
#747=FACE_OUTER_BOUND('',#1019,.T.);
#748=FACE_OUTER_BOUND('',#1020,.T.);
#749=FACE_OUTER_BOUND('',#1021,.T.);
#750=FACE_OUTER_BOUND('',#1022,.T.);
#751=FACE_OUTER_BOUND('',#1023,.T.);
#752=FACE_OUTER_BOUND('',#1024,.T.);
#753=FACE_OUTER_BOUND('',#1029,.T.);
#754=FACE_OUTER_BOUND('',#1034,.T.);
#755=FACE_OUTER_BOUND('',#1035,.T.);
#756=FACE_OUTER_BOUND('',#1036,.T.);
#757=FACE_OUTER_BOUND('',#1037,.T.);
#758=FACE_OUTER_BOUND('',#1038,.T.);
#759=FACE_OUTER_BOUND('',#1039,.T.);
#760=FACE_OUTER_BOUND('',#1040,.T.);
#761=FACE_OUTER_BOUND('',#1041,.T.);
#762=FACE_OUTER_BOUND('',#1042,.T.);
#763=FACE_OUTER_BOUND('',#1043,.T.);
#764=FACE_OUTER_BOUND('',#1044,.T.);
#765=FACE_OUTER_BOUND('',#1045,.T.);
#766=FACE_OUTER_BOUND('',#1046,.T.);
#767=FACE_OUTER_BOUND('',#1047,.T.);
#768=FACE_OUTER_BOUND('',#1048,.T.);
#769=FACE_OUTER_BOUND('',#1049,.T.);
#770=FACE_OUTER_BOUND('',#1050,.T.);
#771=FACE_OUTER_BOUND('',#1051,.T.);
#772=FACE_OUTER_BOUND('',#1052,.T.);
#773=FACE_OUTER_BOUND('',#1053,.T.);
#774=FACE_OUTER_BOUND('',#1054,.T.);
#775=FACE_OUTER_BOUND('',#1059,.T.);
#776=FACE_OUTER_BOUND('',#1064,.T.);
#777=FACE_OUTER_BOUND('',#1065,.T.);
#778=FACE_OUTER_BOUND('',#1066,.T.);
#779=FACE_OUTER_BOUND('',#1068,.T.);
#780=FACE_OUTER_BOUND('',#1070,.T.);
#781=FACE_OUTER_BOUND('',#1071,.T.);
#782=FACE_OUTER_BOUND('',#1072,.T.);
#783=FACE_OUTER_BOUND('',#1074,.T.);
#784=FACE_OUTER_BOUND('',#1076,.T.);
#785=FACE_OUTER_BOUND('',#1077,.T.);
#786=FACE_OUTER_BOUND('',#1078,.T.);
#787=FACE_OUTER_BOUND('',#1079,.T.);
#788=FACE_OUTER_BOUND('',#1080,.T.);
#789=FACE_OUTER_BOUND('',#1081,.T.);
#790=FACE_OUTER_BOUND('',#1082,.T.);
#791=FACE_OUTER_BOUND('',#1083,.T.);
#792=FACE_OUTER_BOUND('',#1084,.T.);
#793=FACE_OUTER_BOUND('',#1089,.T.);
#794=FACE_OUTER_BOUND('',#1094,.T.);
#795=FACE_OUTER_BOUND('',#1095,.T.);
#796=FACE_OUTER_BOUND('',#1096,.T.);
#797=FACE_OUTER_BOUND('',#1098,.T.);
#798=FACE_OUTER_BOUND('',#1100,.T.);
#799=FACE_OUTER_BOUND('',#1101,.T.);
#800=FACE_OUTER_BOUND('',#1102,.T.);
#801=FACE_OUTER_BOUND('',#1104,.T.);
#802=FACE_OUTER_BOUND('',#1106,.T.);
#803=FACE_OUTER_BOUND('',#1107,.T.);
#804=FACE_OUTER_BOUND('',#1108,.T.);
#805=FACE_OUTER_BOUND('',#1111,.T.);
#806=FACE_OUTER_BOUND('',#1112,.T.);
#807=FACE_OUTER_BOUND('',#1113,.T.);
#808=FACE_OUTER_BOUND('',#1114,.T.);
#809=FACE_OUTER_BOUND('',#1115,.T.);
#810=FACE_OUTER_BOUND('',#1116,.T.);
#811=FACE_OUTER_BOUND('',#1117,.T.);
#812=FACE_OUTER_BOUND('',#1121,.T.);
#813=FACE_OUTER_BOUND('',#1122,.T.);
#814=FACE_OUTER_BOUND('',#1124,.T.);
#815=FACE_OUTER_BOUND('',#1126,.T.);
#816=FACE_OUTER_BOUND('',#1127,.T.);
#817=FACE_OUTER_BOUND('',#1128,.T.);
#818=FACE_OUTER_BOUND('',#1129,.T.);
#819=FACE_OUTER_BOUND('',#1130,.T.);
#820=FACE_OUTER_BOUND('',#1131,.T.);
#821=FACE_OUTER_BOUND('',#1132,.T.);
#822=FACE_OUTER_BOUND('',#1133,.T.);
#823=FACE_OUTER_BOUND('',#1134,.T.);
#824=FACE_OUTER_BOUND('',#1135,.T.);
#825=FACE_OUTER_BOUND('',#1136,.T.);
#826=FACE_OUTER_BOUND('',#1137,.T.);
#827=FACE_OUTER_BOUND('',#1141,.T.);
#828=FACE_OUTER_BOUND('',#1142,.T.);
#829=FACE_OUTER_BOUND('',#1144,.T.);
#830=FACE_OUTER_BOUND('',#1147,.T.);
#831=FACE_OUTER_BOUND('',#1149,.T.);
#832=FACE_OUTER_BOUND('',#1150,.T.);
#833=FACE_OUTER_BOUND('',#1151,.T.);
#834=FACE_OUTER_BOUND('',#1158,.T.);
#835=FACE_OUTER_BOUND('',#1159,.T.);
#836=FACE_OUTER_BOUND('',#1160,.T.);
#837=FACE_OUTER_BOUND('',#1161,.T.);
#838=FACE_OUTER_BOUND('',#1162,.T.);
#839=FACE_OUTER_BOUND('',#1164,.T.);
#840=FACE_OUTER_BOUND('',#1166,.T.);
#841=FACE_OUTER_BOUND('',#1167,.T.);
#842=FACE_OUTER_BOUND('',#1169,.T.);
#843=FACE_OUTER_BOUND('',#1176,.T.);
#844=FACE_OUTER_BOUND('',#1177,.T.);
#845=FACE_OUTER_BOUND('',#1178,.T.);
#846=FACE_OUTER_BOUND('',#1180,.T.);
#847=FACE_OUTER_BOUND('',#1182,.T.);
#848=FACE_OUTER_BOUND('',#1183,.T.);
#849=FACE_OUTER_BOUND('',#1184,.T.);
#850=FACE_OUTER_BOUND('',#1185,.T.);
#851=FACE_OUTER_BOUND('',#1186,.T.);
#852=FACE_OUTER_BOUND('',#1187,.T.);
#853=FACE_OUTER_BOUND('',#1188,.T.);
#854=FACE_OUTER_BOUND('',#1189,.T.);
#855=FACE_OUTER_BOUND('',#1190,.T.);
#856=FACE_OUTER_BOUND('',#1191,.T.);
#857=FACE_OUTER_BOUND('',#1192,.T.);
#858=FACE_OUTER_BOUND('',#1193,.T.);
#859=FACE_OUTER_BOUND('',#1194,.T.);
#860=FACE_OUTER_BOUND('',#1195,.T.);
#861=FACE_OUTER_BOUND('',#1197,.T.);
#862=FACE_OUTER_BOUND('',#1198,.T.);
#863=FACE_OUTER_BOUND('',#1199,.T.);
#864=FACE_OUTER_BOUND('',#1200,.T.);
#865=FACE_OUTER_BOUND('',#1201,.T.);
#866=FACE_OUTER_BOUND('',#1202,.T.);
#867=FACE_OUTER_BOUND('',#1203,.T.);
#868=FACE_OUTER_BOUND('',#1204,.T.);
#869=FACE_OUTER_BOUND('',#1205,.T.);
#870=FACE_OUTER_BOUND('',#1206,.T.);
#871=FACE_OUTER_BOUND('',#1208,.T.);
#872=FACE_OUTER_BOUND('',#1209,.T.);
#873=FACE_OUTER_BOUND('',#1211,.T.);
#874=FACE_OUTER_BOUND('',#1212,.T.);
#875=FACE_OUTER_BOUND('',#1213,.T.);
#876=FACE_OUTER_BOUND('',#1214,.T.);
#877=FACE_OUTER_BOUND('',#1215,.T.);
#878=FACE_OUTER_BOUND('',#1216,.T.);
#879=FACE_OUTER_BOUND('',#1217,.T.);
#880=FACE_OUTER_BOUND('',#1218,.T.);
#881=FACE_OUTER_BOUND('',#1219,.T.);
#882=FACE_OUTER_BOUND('',#1220,.T.);
#883=FACE_OUTER_BOUND('',#1221,.T.);
#884=FACE_OUTER_BOUND('',#1223,.T.);
#885=FACE_OUTER_BOUND('',#1224,.T.);
#886=FACE_OUTER_BOUND('',#1226,.T.);
#887=FACE_OUTER_BOUND('',#1232,.T.);
#888=FACE_OUTER_BOUND('',#1233,.T.);
#889=FACE_OUTER_BOUND('',#1235,.T.);
#890=FACE_OUTER_BOUND('',#1237,.T.);
#891=FACE_OUTER_BOUND('',#1243,.T.);
#892=FACE_OUTER_BOUND('',#1244,.T.);
#893=FACE_OUTER_BOUND('',#1245,.T.);
#894=FACE_OUTER_BOUND('',#1247,.T.);
#895=FACE_OUTER_BOUND('',#1249,.T.);
#896=FACE_OUTER_BOUND('',#1250,.T.);
#897=FACE_OUTER_BOUND('',#1251,.T.);
#898=FACE_OUTER_BOUND('',#1252,.T.);
#899=FACE_OUTER_BOUND('',#1253,.T.);
#900=FACE_OUTER_BOUND('',#1254,.T.);
#901=FACE_OUTER_BOUND('',#1255,.T.);
#902=FACE_OUTER_BOUND('',#1256,.T.);
#903=FACE_OUTER_BOUND('',#1258,.T.);
#904=FACE_OUTER_BOUND('',#1260,.T.);
#905=FACE_OUTER_BOUND('',#1261,.T.);
#906=FACE_OUTER_BOUND('',#1262,.T.);
#907=FACE_OUTER_BOUND('',#1263,.T.);
#908=FACE_OUTER_BOUND('',#1264,.T.);
#909=FACE_OUTER_BOUND('',#1265,.T.);
#910=FACE_OUTER_BOUND('',#1266,.T.);
#911=FACE_OUTER_BOUND('',#1267,.T.);
#912=FACE_OUTER_BOUND('',#1268,.T.);
#913=FACE_OUTER_BOUND('',#1269,.T.);
#914=FACE_OUTER_BOUND('',#1270,.T.);
#915=FACE_OUTER_BOUND('',#1271,.T.);
#916=FACE_OUTER_BOUND('',#1273,.T.);
#917=FACE_OUTER_BOUND('',#1275,.T.);
#918=FACE_OUTER_BOUND('',#1276,.T.);
#919=FACE_OUTER_BOUND('',#1282,.T.);
#920=FACE_OUTER_BOUND('',#1283,.T.);
#921=FACE_OUTER_BOUND('',#1285,.T.);
#922=FACE_OUTER_BOUND('',#1287,.T.);
#923=FACE_OUTER_BOUND('',#1293,.T.);
#924=FACE_OUTER_BOUND('',#1294,.T.);
#925=FACE_OUTER_BOUND('',#1295,.T.);
#926=FACE_OUTER_BOUND('',#1297,.T.);
#927=FACE_OUTER_BOUND('',#1299,.T.);
#928=FACE_OUTER_BOUND('',#1300,.T.);
#929=FACE_OUTER_BOUND('',#1301,.T.);
#930=FACE_OUTER_BOUND('',#1303,.T.);
#931=FACE_OUTER_BOUND('',#1305,.T.);
#932=FACE_OUTER_BOUND('',#1306,.T.);
#933=FACE_OUTER_BOUND('',#1307,.T.);
#934=FACE_OUTER_BOUND('',#1308,.T.);
#935=FACE_OUTER_BOUND('',#1310,.T.);
#936=FACE_OUTER_BOUND('',#1312,.T.);
#937=FACE_OUTER_BOUND('',#1314,.T.);
#938=FACE_OUTER_BOUND('',#1316,.T.);
#939=FACE_OUTER_BOUND('',#1317,.T.);
#940=FACE_OUTER_BOUND('',#1318,.T.);
#941=FACE_OUTER_BOUND('',#1319,.T.);
#942=FACE_OUTER_BOUND('',#1321,.T.);
#943=FACE_OUTER_BOUND('',#1323,.T.);
#944=FACE_OUTER_BOUND('',#1325,.T.);
#945=FACE_OUTER_BOUND('',#1327,.T.);
#946=FACE_OUTER_BOUND('',#1328,.T.);
#947=FACE_OUTER_BOUND('',#1329,.T.);
#948=FACE_OUTER_BOUND('',#1330,.T.);
#949=FACE_OUTER_BOUND('',#1331,.T.);
#950=FACE_OUTER_BOUND('',#1332,.T.);
#951=FACE_OUTER_BOUND('',#1333,.T.);
#952=FACE_OUTER_BOUND('',#1334,.T.);
#953=FACE_OUTER_BOUND('',#1335,.T.);
#954=FACE_OUTER_BOUND('',#1336,.T.);
#955=FACE_OUTER_BOUND('',#1337,.T.);
#956=FACE_OUTER_BOUND('',#1338,.T.);
#957=FACE_OUTER_BOUND('',#1339,.T.);
#958=FACE_OUTER_BOUND('',#1340,.T.);
#959=FACE_OUTER_BOUND('',#1341,.T.);
#960=FACE_OUTER_BOUND('',#1343,.T.);
#961=FACE_OUTER_BOUND('',#1344,.T.);
#962=FACE_OUTER_BOUND('',#1345,.T.);
#963=FACE_OUTER_BOUND('',#1346,.T.);
#964=FACE_OUTER_BOUND('',#1347,.T.);
#965=FACE_OUTER_BOUND('',#1348,.T.);
#966=FACE_OUTER_BOUND('',#1349,.T.);
#967=FACE_OUTER_BOUND('',#1350,.T.);
#968=FACE_OUTER_BOUND('',#1351,.T.);
#969=FACE_OUTER_BOUND('',#1352,.T.);
#970=FACE_OUTER_BOUND('',#1353,.T.);
#971=FACE_OUTER_BOUND('',#1354,.T.);
#972=FACE_OUTER_BOUND('',#1355,.T.);
#973=FACE_OUTER_BOUND('',#1356,.T.);
#974=FACE_OUTER_BOUND('',#1357,.T.);
#975=FACE_OUTER_BOUND('',#1358,.T.);
#976=FACE_OUTER_BOUND('',#1359,.T.);
#977=FACE_OUTER_BOUND('',#1361,.T.);
#978=FACE_OUTER_BOUND('',#1362,.T.);
#979=FACE_OUTER_BOUND('',#1363,.T.);
#980=FACE_OUTER_BOUND('',#1364,.T.);
#981=FACE_OUTER_BOUND('',#1365,.T.);
#982=FACE_OUTER_BOUND('',#1366,.T.);
#983=FACE_OUTER_BOUND('',#1367,.T.);
#984=FACE_OUTER_BOUND('',#1368,.T.);
#985=FACE_OUTER_BOUND('',#1369,.T.);
#986=FACE_OUTER_BOUND('',#1370,.T.);
#987=FACE_OUTER_BOUND('',#1371,.T.);
#988=FACE_OUTER_BOUND('',#1372,.T.);
#989=FACE_OUTER_BOUND('',#1373,.T.);
#990=FACE_OUTER_BOUND('',#1374,.T.);
#991=FACE_OUTER_BOUND('',#1375,.T.);
#992=FACE_OUTER_BOUND('',#1377,.T.);
#993=FACE_OUTER_BOUND('',#1379,.T.);
#994=FACE_OUTER_BOUND('',#1380,.T.);
#995=FACE_OUTER_BOUND('',#1381,.T.);
#996=FACE_OUTER_BOUND('',#1382,.T.);
#997=FACE_OUTER_BOUND('',#1383,.T.);
#998=FACE_OUTER_BOUND('',#1384,.T.);
#999=FACE_OUTER_BOUND('',#1385,.T.);
#1000=FACE_OUTER_BOUND('',#1386,.T.);
#1001=FACE_OUTER_BOUND('',#1387,.T.);
#1002=FACE_OUTER_BOUND('',#1388,.T.);
#1003=FACE_OUTER_BOUND('',#1390,.T.);
#1004=FACE_OUTER_BOUND('',#1392,.T.);
#1005=FACE_OUTER_BOUND('',#1393,.T.);
#1006=FACE_OUTER_BOUND('',#1394,.T.);
#1007=FACE_OUTER_BOUND('',#1395,.T.);
#1008=FACE_OUTER_BOUND('',#1396,.T.);
#1009=FACE_OUTER_BOUND('',#1397,.T.);
#1010=FACE_OUTER_BOUND('',#1398,.T.);
#1011=FACE_OUTER_BOUND('',#1399,.T.);
#1012=FACE_OUTER_BOUND('',#1401,.T.);
#1013=FACE_OUTER_BOUND('',#1402,.T.);
#1014=FACE_OUTER_BOUND('',#1403,.T.);
#1015=FACE_OUTER_BOUND('',#1404,.T.);
#1016=EDGE_LOOP('',(#3243,#3244,#3245,#3246));
#1017=EDGE_LOOP('',(#3247,#3248,#3249,#3250));
#1018=EDGE_LOOP('',(#3251,#3252,#3253,#3254));
#1019=EDGE_LOOP('',(#3255,#3256,#3257,#3258));
#1020=EDGE_LOOP('',(#3259,#3260,#3261,#3262));
#1021=EDGE_LOOP('',(#3263,#3264,#3265,#3266));
#1022=EDGE_LOOP('',(#3267,#3268,#3269,#3270));
#1023=EDGE_LOOP('',(#3271,#3272,#3273,#3274));
#1024=EDGE_LOOP('',(#3275,#3276,#3277,#3278));
#1025=EDGE_LOOP('',(#3279));
#1026=EDGE_LOOP('',(#3280));
#1027=EDGE_LOOP('',(#3281));
#1028=EDGE_LOOP('',(#3282));
#1029=EDGE_LOOP('',(#3283,#3284,#3285,#3286));
#1030=EDGE_LOOP('',(#3287));
#1031=EDGE_LOOP('',(#3288));
#1032=EDGE_LOOP('',(#3289));
#1033=EDGE_LOOP('',(#3290));
#1034=EDGE_LOOP('',(#3291,#3292,#3293,#3294));
#1035=EDGE_LOOP('',(#3295,#3296,#3297,#3298));
#1036=EDGE_LOOP('',(#3299,#3300,#3301,#3302));
#1037=EDGE_LOOP('',(#3303,#3304,#3305,#3306));
#1038=EDGE_LOOP('',(#3307,#3308,#3309,#3310));
#1039=EDGE_LOOP('',(#3311,#3312,#3313,#3314));
#1040=EDGE_LOOP('',(#3315,#3316,#3317,#3318));
#1041=EDGE_LOOP('',(#3319,#3320,#3321,#3322));
#1042=EDGE_LOOP('',(#3323,#3324,#3325,#3326));
#1043=EDGE_LOOP('',(#3327,#3328,#3329,#3330));
#1044=EDGE_LOOP('',(#3331,#3332,#3333,#3334));
#1045=EDGE_LOOP('',(#3335,#3336,#3337,#3338));
#1046=EDGE_LOOP('',(#3339,#3340,#3341,#3342));
#1047=EDGE_LOOP('',(#3343,#3344,#3345,#3346));
#1048=EDGE_LOOP('',(#3347,#3348,#3349,#3350));
#1049=EDGE_LOOP('',(#3351,#3352,#3353,#3354));
#1050=EDGE_LOOP('',(#3355,#3356,#3357,#3358));
#1051=EDGE_LOOP('',(#3359,#3360,#3361,#3362));
#1052=EDGE_LOOP('',(#3363,#3364,#3365,#3366));
#1053=EDGE_LOOP('',(#3367,#3368,#3369,#3370));
#1054=EDGE_LOOP('',(#3371,#3372,#3373,#3374));
#1055=EDGE_LOOP('',(#3375));
#1056=EDGE_LOOP('',(#3376));
#1057=EDGE_LOOP('',(#3377));
#1058=EDGE_LOOP('',(#3378));
#1059=EDGE_LOOP('',(#3379,#3380,#3381,#3382));
#1060=EDGE_LOOP('',(#3383));
#1061=EDGE_LOOP('',(#3384));
#1062=EDGE_LOOP('',(#3385));
#1063=EDGE_LOOP('',(#3386));
#1064=EDGE_LOOP('',(#3387,#3388,#3389,#3390));
#1065=EDGE_LOOP('',(#3391,#3392,#3393,#3394));
#1066=EDGE_LOOP('',(#3395));
#1067=EDGE_LOOP('',(#3396));
#1068=EDGE_LOOP('',(#3397));
#1069=EDGE_LOOP('',(#3398));
#1070=EDGE_LOOP('',(#3399,#3400,#3401,#3402));
#1071=EDGE_LOOP('',(#3403,#3404,#3405,#3406));
#1072=EDGE_LOOP('',(#3407));
#1073=EDGE_LOOP('',(#3408));
#1074=EDGE_LOOP('',(#3409));
#1075=EDGE_LOOP('',(#3410));
#1076=EDGE_LOOP('',(#3411,#3412,#3413,#3414));
#1077=EDGE_LOOP('',(#3415,#3416,#3417,#3418));
#1078=EDGE_LOOP('',(#3419,#3420,#3421,#3422));
#1079=EDGE_LOOP('',(#3423,#3424,#3425,#3426));
#1080=EDGE_LOOP('',(#3427,#3428,#3429,#3430));
#1081=EDGE_LOOP('',(#3431,#3432,#3433,#3434));
#1082=EDGE_LOOP('',(#3435,#3436,#3437,#3438));
#1083=EDGE_LOOP('',(#3439,#3440,#3441,#3442));
#1084=EDGE_LOOP('',(#3443,#3444,#3445,#3446));
#1085=EDGE_LOOP('',(#3447));
#1086=EDGE_LOOP('',(#3448));
#1087=EDGE_LOOP('',(#3449));
#1088=EDGE_LOOP('',(#3450));
#1089=EDGE_LOOP('',(#3451,#3452,#3453,#3454));
#1090=EDGE_LOOP('',(#3455));
#1091=EDGE_LOOP('',(#3456));
#1092=EDGE_LOOP('',(#3457));
#1093=EDGE_LOOP('',(#3458));
#1094=EDGE_LOOP('',(#3459,#3460,#3461,#3462));
#1095=EDGE_LOOP('',(#3463,#3464,#3465,#3466));
#1096=EDGE_LOOP('',(#3467));
#1097=EDGE_LOOP('',(#3468));
#1098=EDGE_LOOP('',(#3469));
#1099=EDGE_LOOP('',(#3470));
#1100=EDGE_LOOP('',(#3471,#3472,#3473,#3474));
#1101=EDGE_LOOP('',(#3475,#3476,#3477,#3478));
#1102=EDGE_LOOP('',(#3479));
#1103=EDGE_LOOP('',(#3480));
#1104=EDGE_LOOP('',(#3481));
#1105=EDGE_LOOP('',(#3482));
#1106=EDGE_LOOP('',(#3483,#3484,#3485,#3486));
#1107=EDGE_LOOP('',(#3487,#3488,#3489,#3490));
#1108=EDGE_LOOP('',(#3491,#3492));
#1109=EDGE_LOOP('',(#3493));
#1110=EDGE_LOOP('',(#3494));
#1111=EDGE_LOOP('',(#3495,#3496,#3497));
#1112=EDGE_LOOP('',(#3498,#3499,#3500));
#1113=EDGE_LOOP('',(#3501,#3502,#3503));
#1114=EDGE_LOOP('',(#3504,#3505,#3506,#3507));
#1115=EDGE_LOOP('',(#3508,#3509,#3510));
#1116=EDGE_LOOP('',(#3511,#3512,#3513,#3514));
#1117=EDGE_LOOP('',(#3515,#3516,#3517,#3518));
#1118=EDGE_LOOP('',(#3519));
#1119=EDGE_LOOP('',(#3520));
#1120=EDGE_LOOP('',(#3521,#3522,#3523,#3524,#3525,#3526,#3527,#3528,#3529,
#3530,#3531,#3532));
#1121=EDGE_LOOP('',(#3533,#3534,#3535,#3536,#3537,#3538,#3539,#3540,#3541,
#3542,#3543,#3544));
#1122=EDGE_LOOP('',(#3545,#3546));
#1123=EDGE_LOOP('',(#3547));
#1124=EDGE_LOOP('',(#3548,#3549));
#1125=EDGE_LOOP('',(#3550));
#1126=EDGE_LOOP('',(#3551,#3552,#3553,#3554));
#1127=EDGE_LOOP('',(#3555,#3556,#3557,#3558));
#1128=EDGE_LOOP('',(#3559,#3560,#3561,#3562));
#1129=EDGE_LOOP('',(#3563,#3564,#3565,#3566));
#1130=EDGE_LOOP('',(#3567,#3568,#3569,#3570));
#1131=EDGE_LOOP('',(#3571,#3572,#3573,#3574));
#1132=EDGE_LOOP('',(#3575,#3576,#3577,#3578));
#1133=EDGE_LOOP('',(#3579,#3580,#3581,#3582));
#1134=EDGE_LOOP('',(#3583,#3584,#3585,#3586));
#1135=EDGE_LOOP('',(#3587,#3588,#3589,#3590));
#1136=EDGE_LOOP('',(#3591,#3592,#3593,#3594));
#1137=EDGE_LOOP('',(#3595,#3596,#3597,#3598));
#1138=EDGE_LOOP('',(#3599,#3600,#3601,#3602));
#1139=EDGE_LOOP('',(#3603));
#1140=EDGE_LOOP('',(#3604));
#1141=EDGE_LOOP('',(#3605,#3606,#3607,#3608));
#1142=EDGE_LOOP('',(#3609));
#1143=EDGE_LOOP('',(#3610));
#1144=EDGE_LOOP('',(#3611,#3612));
#1145=EDGE_LOOP('',(#3613));
#1146=EDGE_LOOP('',(#3614));
#1147=EDGE_LOOP('',(#3615));
#1148=EDGE_LOOP('',(#3616));
#1149=EDGE_LOOP('',(#3617,#3618,#3619,#3620,#3621,#3622));
#1150=EDGE_LOOP('',(#3623,#3624,#3625,#3626,#3627,#3628));
#1151=EDGE_LOOP('',(#3629,#3630,#3631,#3632));
#1152=EDGE_LOOP('',(#3633,#3634,#3635));
#1153=EDGE_LOOP('',(#3636,#3637,#3638));
#1154=EDGE_LOOP('',(#3639,#3640,#3641));
#1155=EDGE_LOOP('',(#3642,#3643,#3644));
#1156=EDGE_LOOP('',(#3645,#3646,#3647));
#1157=EDGE_LOOP('',(#3648,#3649,#3650));
#1158=EDGE_LOOP('',(#3651,#3652,#3653,#3654,#3655,#3656));
#1159=EDGE_LOOP('',(#3657,#3658,#3659,#3660,#3661,#3662));
#1160=EDGE_LOOP('',(#3663,#3664,#3665,#3666,#3667,#3668));
#1161=EDGE_LOOP('',(#3669,#3670,#3671,#3672,#3673,#3674));
#1162=EDGE_LOOP('',(#3675));
#1163=EDGE_LOOP('',(#3676));
#1164=EDGE_LOOP('',(#3677));
#1165=EDGE_LOOP('',(#3678));
#1166=EDGE_LOOP('',(#3679,#3680,#3681,#3682));
#1167=EDGE_LOOP('',(#3683));
#1168=EDGE_LOOP('',(#3684));
#1169=EDGE_LOOP('',(#3685,#3686,#3687,#3688));
#1170=EDGE_LOOP('',(#3689));
#1171=EDGE_LOOP('',(#3690));
#1172=EDGE_LOOP('',(#3691));
#1173=EDGE_LOOP('',(#3692));
#1174=EDGE_LOOP('',(#3693));
#1175=EDGE_LOOP('',(#3694));
#1176=EDGE_LOOP('',(#3695,#3696,#3697,#3698));
#1177=EDGE_LOOP('',(#3699,#3700,#3701,#3702));
#1178=EDGE_LOOP('',(#3703));
#1179=EDGE_LOOP('',(#3704));
#1180=EDGE_LOOP('',(#3705));
#1181=EDGE_LOOP('',(#3706));
#1182=EDGE_LOOP('',(#3707,#3708,#3709,#3710));
#1183=EDGE_LOOP('',(#3711,#3712,#3713,#3714));
#1184=EDGE_LOOP('',(#3715,#3716,#3717,#3718));
#1185=EDGE_LOOP('',(#3719,#3720,#3721,#3722));
#1186=EDGE_LOOP('',(#3723,#3724,#3725,#3726));
#1187=EDGE_LOOP('',(#3727,#3728,#3729,#3730));
#1188=EDGE_LOOP('',(#3731,#3732,#3733,#3734,#3735,#3736));
#1189=EDGE_LOOP('',(#3737,#3738,#3739,#3740,#3741,#3742));
#1190=EDGE_LOOP('',(#3743));
#1191=EDGE_LOOP('',(#3744));
#1192=EDGE_LOOP('',(#3745,#3746,#3747,#3748));
#1193=EDGE_LOOP('',(#3749,#3750,#3751,#3752));
#1194=EDGE_LOOP('',(#3753,#3754,#3755,#3756));
#1195=EDGE_LOOP('',(#3757));
#1196=EDGE_LOOP('',(#3758));
#1197=EDGE_LOOP('',(#3759,#3760,#3761,#3762));
#1198=EDGE_LOOP('',(#3763,#3764,#3765,#3766));
#1199=EDGE_LOOP('',(#3767,#3768,#3769,#3770));
#1200=EDGE_LOOP('',(#3771));
#1201=EDGE_LOOP('',(#3772,#3773,#3774,#3775));
#1202=EDGE_LOOP('',(#3776,#3777,#3778,#3779));
#1203=EDGE_LOOP('',(#3780,#3781,#3782,#3783));
#1204=EDGE_LOOP('',(#3784,#3785,#3786,#3787));
#1205=EDGE_LOOP('',(#3788,#3789,#3790,#3791));
#1206=EDGE_LOOP('',(#3792,#3793,#3794,#3795));
#1207=EDGE_LOOP('',(#3796,#3797,#3798,#3799));
#1208=EDGE_LOOP('',(#3800));
#1209=EDGE_LOOP('',(#3801));
#1210=EDGE_LOOP('',(#3802));
#1211=EDGE_LOOP('',(#3803,#3804,#3805,#3806));
#1212=EDGE_LOOP('',(#3807,#3808,#3809,#3810));
#1213=EDGE_LOOP('',(#3811,#3812,#3813,#3814));
#1214=EDGE_LOOP('',(#3815,#3816,#3817,#3818));
#1215=EDGE_LOOP('',(#3819,#3820));
#1216=EDGE_LOOP('',(#3821,#3822,#3823,#3824,#3825,#3826,#3827,#3828,#3829));
#1217=EDGE_LOOP('',(#3830,#3831,#3832));
#1218=EDGE_LOOP('',(#3833,#3834,#3835,#3836));
#1219=EDGE_LOOP('',(#3837,#3838,#3839,#3840));
#1220=EDGE_LOOP('',(#3841,#3842,#3843,#3844));
#1221=EDGE_LOOP('',(#3845));
#1222=EDGE_LOOP('',(#3846,#3847,#3848,#3849));
#1223=EDGE_LOOP('',(#3850,#3851,#3852,#3853));
#1224=EDGE_LOOP('',(#3854));
#1225=EDGE_LOOP('',(#3855,#3856,#3857,#3858));
#1226=EDGE_LOOP('',(#3859));
#1227=EDGE_LOOP('',(#3860));
#1228=EDGE_LOOP('',(#3861));
#1229=EDGE_LOOP('',(#3862));
#1230=EDGE_LOOP('',(#3863));
#1231=EDGE_LOOP('',(#3864));
#1232=EDGE_LOOP('',(#3865,#3866,#3867,#3868));
#1233=EDGE_LOOP('',(#3869,#3870,#3871,#3872));
#1234=EDGE_LOOP('',(#3873,#3874,#3875,#3876));
#1235=EDGE_LOOP('',(#3877,#3878,#3879,#3880));
#1236=EDGE_LOOP('',(#3881,#3882));
#1237=EDGE_LOOP('',(#3883));
#1238=EDGE_LOOP('',(#3884));
#1239=EDGE_LOOP('',(#3885));
#1240=EDGE_LOOP('',(#3886));
#1241=EDGE_LOOP('',(#3887));
#1242=EDGE_LOOP('',(#3888));
#1243=EDGE_LOOP('',(#3889,#3890,#3891,#3892));
#1244=EDGE_LOOP('',(#3893,#3894,#3895,#3896));
#1245=EDGE_LOOP('',(#3897));
#1246=EDGE_LOOP('',(#3898));
#1247=EDGE_LOOP('',(#3899));
#1248=EDGE_LOOP('',(#3900));
#1249=EDGE_LOOP('',(#3901,#3902,#3903,#3904));
#1250=EDGE_LOOP('',(#3905));
#1251=EDGE_LOOP('',(#3906,#3907,#3908,#3909));
#1252=EDGE_LOOP('',(#3910,#3911,#3912,#3913));
#1253=EDGE_LOOP('',(#3914,#3915,#3916,#3917));
#1254=EDGE_LOOP('',(#3918,#3919,#3920,#3921));
#1255=EDGE_LOOP('',(#3922,#3923,#3924,#3925));
#1256=EDGE_LOOP('',(#3926,#3927,#3928,#3929));
#1257=EDGE_LOOP('',(#3930,#3931,#3932,#3933));
#1258=EDGE_LOOP('',(#3934));
#1259=EDGE_LOOP('',(#3935));
#1260=EDGE_LOOP('',(#3936));
#1261=EDGE_LOOP('',(#3937,#3938,#3939,#3940));
#1262=EDGE_LOOP('',(#3941,#3942,#3943,#3944));
#1263=EDGE_LOOP('',(#3945,#3946,#3947,#3948));
#1264=EDGE_LOOP('',(#3949,#3950,#3951,#3952));
#1265=EDGE_LOOP('',(#3953,#3954));
#1266=EDGE_LOOP('',(#3955,#3956,#3957,#3958,#3959,#3960,#3961,#3962,#3963));
#1267=EDGE_LOOP('',(#3964,#3965,#3966));
#1268=EDGE_LOOP('',(#3967,#3968,#3969,#3970));
#1269=EDGE_LOOP('',(#3971,#3972,#3973,#3974));
#1270=EDGE_LOOP('',(#3975,#3976,#3977,#3978));
#1271=EDGE_LOOP('',(#3979));
#1272=EDGE_LOOP('',(#3980,#3981,#3982,#3983));
#1273=EDGE_LOOP('',(#3984,#3985,#3986,#3987));
#1274=EDGE_LOOP('',(#3988,#3989,#3990,#3991));
#1275=EDGE_LOOP('',(#3992,#3993,#3994,#3995));
#1276=EDGE_LOOP('',(#3996));
#1277=EDGE_LOOP('',(#3997));
#1278=EDGE_LOOP('',(#3998));
#1279=EDGE_LOOP('',(#3999));
#1280=EDGE_LOOP('',(#4000));
#1281=EDGE_LOOP('',(#4001));
#1282=EDGE_LOOP('',(#4002,#4003,#4004,#4005));
#1283=EDGE_LOOP('',(#4006,#4007,#4008,#4009));
#1284=EDGE_LOOP('',(#4010,#4011));
#1285=EDGE_LOOP('',(#4012));
#1286=EDGE_LOOP('',(#4013,#4014,#4015,#4016));
#1287=EDGE_LOOP('',(#4017));
#1288=EDGE_LOOP('',(#4018));
#1289=EDGE_LOOP('',(#4019));
#1290=EDGE_LOOP('',(#4020));
#1291=EDGE_LOOP('',(#4021));
#1292=EDGE_LOOP('',(#4022));
#1293=EDGE_LOOP('',(#4023,#4024,#4025,#4026));
#1294=EDGE_LOOP('',(#4027,#4028,#4029,#4030));
#1295=EDGE_LOOP('',(#4031));
#1296=EDGE_LOOP('',(#4032));
#1297=EDGE_LOOP('',(#4033));
#1298=EDGE_LOOP('',(#4034));
#1299=EDGE_LOOP('',(#4035,#4036,#4037,#4038));
#1300=EDGE_LOOP('',(#4039,#4040,#4041,#4042));
#1301=EDGE_LOOP('',(#4043));
#1302=EDGE_LOOP('',(#4044));
#1303=EDGE_LOOP('',(#4045));
#1304=EDGE_LOOP('',(#4046));
#1305=EDGE_LOOP('',(#4047,#4048));
#1306=EDGE_LOOP('',(#4049,#4050,#4051,#4052,#4053,#4054,#4055,#4056,#4057));
#1307=EDGE_LOOP('',(#4058,#4059,#4060));
#1308=EDGE_LOOP('',(#4061,#4062,#4063,#4064));
#1309=EDGE_LOOP('',(#4065,#4066,#4067,#4068));
#1310=EDGE_LOOP('',(#4069,#4070,#4071,#4072));
#1311=EDGE_LOOP('',(#4073,#4074));
#1312=EDGE_LOOP('',(#4075));
#1313=EDGE_LOOP('',(#4076));
#1314=EDGE_LOOP('',(#4077));
#1315=EDGE_LOOP('',(#4078));
#1316=EDGE_LOOP('',(#4079,#4080));
#1317=EDGE_LOOP('',(#4081,#4082,#4083,#4084,#4085,#4086,#4087,#4088,#4089));
#1318=EDGE_LOOP('',(#4090,#4091,#4092));
#1319=EDGE_LOOP('',(#4093,#4094,#4095,#4096));
#1320=EDGE_LOOP('',(#4097,#4098,#4099,#4100));
#1321=EDGE_LOOP('',(#4101,#4102,#4103,#4104));
#1322=EDGE_LOOP('',(#4105,#4106));
#1323=EDGE_LOOP('',(#4107));
#1324=EDGE_LOOP('',(#4108));
#1325=EDGE_LOOP('',(#4109));
#1326=EDGE_LOOP('',(#4110));
#1327=EDGE_LOOP('',(#4111,#4112,#4113,#4114,#4115,#4116,#4117,#4118));
#1328=EDGE_LOOP('',(#4119,#4120,#4121,#4122));
#1329=EDGE_LOOP('',(#4123,#4124,#4125,#4126));
#1330=EDGE_LOOP('',(#4127,#4128,#4129,#4130));
#1331=EDGE_LOOP('',(#4131,#4132,#4133,#4134));
#1332=EDGE_LOOP('',(#4135,#4136,#4137,#4138,#4139,#4140,#4141,#4142));
#1333=EDGE_LOOP('',(#4143,#4144,#4145,#4146));
#1334=EDGE_LOOP('',(#4147,#4148,#4149,#4150));
#1335=EDGE_LOOP('',(#4151,#4152,#4153,#4154));
#1336=EDGE_LOOP('',(#4155,#4156,#4157,#4158));
#1337=EDGE_LOOP('',(#4159));
#1338=EDGE_LOOP('',(#4160,#4161,#4162,#4163));
#1339=EDGE_LOOP('',(#4164,#4165,#4166,#4167));
#1340=EDGE_LOOP('',(#4168,#4169,#4170,#4171));
#1341=EDGE_LOOP('',(#4172));
#1342=EDGE_LOOP('',(#4173));
#1343=EDGE_LOOP('',(#4174,#4175,#4176,#4177));
#1344=EDGE_LOOP('',(#4178,#4179,#4180,#4181));
#1345=EDGE_LOOP('',(#4182,#4183,#4184,#4185));
#1346=EDGE_LOOP('',(#4186));
#1347=EDGE_LOOP('',(#4187,#4188,#4189,#4190));
#1348=EDGE_LOOP('',(#4191,#4192,#4193,#4194));
#1349=EDGE_LOOP('',(#4195,#4196,#4197,#4198));
#1350=EDGE_LOOP('',(#4199,#4200,#4201,#4202));
#1351=EDGE_LOOP('',(#4203,#4204,#4205,#4206));
#1352=EDGE_LOOP('',(#4207,#4208,#4209,#4210));
#1353=EDGE_LOOP('',(#4211,#4212,#4213,#4214,#4215,#4216));
#1354=EDGE_LOOP('',(#4217,#4218,#4219,#4220,#4221,#4222));
#1355=EDGE_LOOP('',(#4223));
#1356=EDGE_LOOP('',(#4224,#4225,#4226,#4227));
#1357=EDGE_LOOP('',(#4228,#4229,#4230,#4231));
#1358=EDGE_LOOP('',(#4232,#4233,#4234,#4235));
#1359=EDGE_LOOP('',(#4236));
#1360=EDGE_LOOP('',(#4237));
#1361=EDGE_LOOP('',(#4238,#4239,#4240,#4241));
#1362=EDGE_LOOP('',(#4242,#4243,#4244,#4245));
#1363=EDGE_LOOP('',(#4246,#4247,#4248,#4249));
#1364=EDGE_LOOP('',(#4250));
#1365=EDGE_LOOP('',(#4251,#4252,#4253,#4254));
#1366=EDGE_LOOP('',(#4255,#4256,#4257,#4258));
#1367=EDGE_LOOP('',(#4259,#4260,#4261,#4262));
#1368=EDGE_LOOP('',(#4263,#4264,#4265,#4266));
#1369=EDGE_LOOP('',(#4267,#4268,#4269,#4270));
#1370=EDGE_LOOP('',(#4271,#4272,#4273,#4274));
#1371=EDGE_LOOP('',(#4275,#4276,#4277,#4278,#4279,#4280));
#1372=EDGE_LOOP('',(#4281,#4282,#4283,#4284,#4285,#4286));
#1373=EDGE_LOOP('',(#4287,#4288,#4289,#4290));
#1374=EDGE_LOOP('',(#4291,#4292,#4293,#4294));
#1375=EDGE_LOOP('',(#4295));
#1376=EDGE_LOOP('',(#4296));
#1377=EDGE_LOOP('',(#4297));
#1378=EDGE_LOOP('',(#4298));
#1379=EDGE_LOOP('',(#4299,#4300,#4301,#4302,#4303,#4304,#4305,#4306,#4307));
#1380=EDGE_LOOP('',(#4308,#4309,#4310,#4311,#4312,#4313,#4314,#4315,#4316));
#1381=EDGE_LOOP('',(#4317,#4318,#4319,#4320));
#1382=EDGE_LOOP('',(#4321,#4322,#4323,#4324));
#1383=EDGE_LOOP('',(#4325,#4326,#4327,#4328));
#1384=EDGE_LOOP('',(#4329,#4330,#4331,#4332));
#1385=EDGE_LOOP('',(#4333,#4334,#4335,#4336));
#1386=EDGE_LOOP('',(#4337,#4338,#4339,#4340));
#1387=EDGE_LOOP('',(#4341,#4342,#4343,#4344));
#1388=EDGE_LOOP('',(#4345));
#1389=EDGE_LOOP('',(#4346));
#1390=EDGE_LOOP('',(#4347));
#1391=EDGE_LOOP('',(#4348));
#1392=EDGE_LOOP('',(#4349,#4350,#4351,#4352));
#1393=EDGE_LOOP('',(#4353,#4354,#4355,#4356));
#1394=EDGE_LOOP('',(#4357,#4358,#4359,#4360));
#1395=EDGE_LOOP('',(#4361,#4362,#4363,#4364));
#1396=EDGE_LOOP('',(#4365,#4366,#4367,#4368));
#1397=EDGE_LOOP('',(#4369,#4370,#4371,#4372));
#1398=EDGE_LOOP('',(#4373,#4374,#4375,#4376,#4377,#4378));
#1399=EDGE_LOOP('',(#4379));
#1400=EDGE_LOOP('',(#4380,#4381,#4382,#4383,#4384,#4385));
#1401=EDGE_LOOP('',(#4386,#4387,#4388,#4389));
#1402=EDGE_LOOP('',(#4390,#4391,#4392,#4393));
#1403=EDGE_LOOP('',(#4394,#4395,#4396,#4397));
#1404=EDGE_LOOP('',(#4398));
#1405=LINE('',#7092,#1750);
#1406=LINE('',#7098,#1751);
#1407=LINE('',#7104,#1752);
#1408=LINE('',#7110,#1753);
#1409=LINE('',#7115,#1754);
#1410=LINE('',#7117,#1755);
#1411=LINE('',#7119,#1756);
#1412=LINE('',#7120,#1757);
#1413=LINE('',#7123,#1758);
#1414=LINE('',#7125,#1759);
#1415=LINE('',#7126,#1760);
#1416=LINE('',#7129,#1761);
#1417=LINE('',#7131,#1762);
#1418=LINE('',#7132,#1763);
#1419=LINE('',#7134,#1764);
#1420=LINE('',#7135,#1765);
#1421=LINE('',#7142,#1766);
#1422=LINE('',#7144,#1767);
#1423=LINE('',#7146,#1768);
#1424=LINE('',#7147,#1769);
#1425=LINE('',#7150,#1770);
#1426=LINE('',#7152,#1771);
#1427=LINE('',#7153,#1772);
#1428=LINE('',#7156,#1773);
#1429=LINE('',#7158,#1774);
#1430=LINE('',#7159,#1775);
#1431=LINE('',#7161,#1776);
#1432=LINE('',#7162,#1777);
#1433=LINE('',#7169,#1778);
#1434=LINE('',#7171,#1779);
#1435=LINE('',#7173,#1780);
#1436=LINE('',#7174,#1781);
#1437=LINE('',#7177,#1782);
#1438=LINE('',#7179,#1783);
#1439=LINE('',#7180,#1784);
#1440=LINE('',#7183,#1785);
#1441=LINE('',#7185,#1786);
#1442=LINE('',#7186,#1787);
#1443=LINE('',#7188,#1788);
#1444=LINE('',#7189,#1789);
#1445=LINE('',#7197,#1790);
#1446=LINE('',#7203,#1791);
#1447=LINE('',#7209,#1792);
#1448=LINE('',#7215,#1793);
#1449=LINE('',#7220,#1794);
#1450=LINE('',#7222,#1795);
#1451=LINE('',#7224,#1796);
#1452=LINE('',#7225,#1797);
#1453=LINE('',#7228,#1798);
#1454=LINE('',#7230,#1799);
#1455=LINE('',#7231,#1800);
#1456=LINE('',#7234,#1801);
#1457=LINE('',#7236,#1802);
#1458=LINE('',#7237,#1803);
#1459=LINE('',#7239,#1804);
#1460=LINE('',#7240,#1805);
#1461=LINE('',#7248,#1806);
#1462=LINE('',#7254,#1807);
#1463=LINE('',#7263,#1808);
#1464=LINE('',#7269,#1809);
#1465=LINE('',#7278,#1810);
#1466=LINE('',#7284,#1811);
#1467=LINE('',#7290,#1812);
#1468=LINE('',#7296,#1813);
#1469=LINE('',#7301,#1814);
#1470=LINE('',#7303,#1815);
#1471=LINE('',#7305,#1816);
#1472=LINE('',#7306,#1817);
#1473=LINE('',#7309,#1818);
#1474=LINE('',#7311,#1819);
#1475=LINE('',#7312,#1820);
#1476=LINE('',#7315,#1821);
#1477=LINE('',#7317,#1822);
#1478=LINE('',#7318,#1823);
#1479=LINE('',#7320,#1824);
#1480=LINE('',#7321,#1825);
#1481=LINE('',#7329,#1826);
#1482=LINE('',#7335,#1827);
#1483=LINE('',#7344,#1828);
#1484=LINE('',#7350,#1829);
#1485=LINE('',#7360,#1830);
#1486=LINE('',#7366,#1831);
#1487=LINE('',#7375,#1832);
#1488=LINE('',#7377,#1833);
#1489=LINE('',#7382,#1834);
#1490=LINE('',#7385,#1835);
#1491=LINE('',#7389,#1836);
#1492=LINE('',#7392,#1837);
#1493=LINE('',#7394,#1838);
#1494=LINE('',#7395,#1839);
#1495=LINE('',#7399,#1840);
#1496=LINE('',#7401,#1841);
#1497=LINE('',#7404,#1842);
#1498=LINE('',#7405,#1843);
#1499=LINE('',#7409,#1844);
#1500=LINE('',#7411,#1845);
#1501=LINE('',#7413,#1846);
#1502=LINE('',#7414,#1847);
#1503=LINE('',#7420,#1848);
#1504=LINE('',#7422,#1849);
#1505=LINE('',#7423,#1850);
#1506=LINE('',#7425,#1851);
#1507=LINE('',#7427,#1852);
#1508=LINE('',#7428,#1853);
#1509=LINE('',#7437,#1854);
#1510=LINE('',#7439,#1855);
#1511=LINE('',#7441,#1856);
#1512=LINE('',#7442,#1857);
#1513=LINE('',#7445,#1858);
#1514=LINE('',#7447,#1859);
#1515=LINE('',#7448,#1860);
#1516=LINE('',#7451,#1861);
#1517=LINE('',#7453,#1862);
#1518=LINE('',#7454,#1863);
#1519=LINE('',#7456,#1864);
#1520=LINE('',#7457,#1865);
#1521=LINE('',#7462,#1866);
#1522=LINE('',#7466,#1867);
#1523=LINE('',#7470,#1868);
#1524=LINE('',#7471,#1869);
#1525=LINE('',#7472,#1870);
#1526=LINE('',#7475,#1871);
#1527=LINE('',#7476,#1872);
#1528=LINE('',#7479,#1873);
#1529=LINE('',#7480,#1874);
#1530=LINE('',#7482,#1875);
#1531=LINE('',#7489,#1876);
#1532=LINE('',#7544,#1877);
#1533=LINE('',#7616,#1878);
#1534=LINE('',#7661,#1879);
#1535=LINE('',#7829,#1880);
#1536=LINE('',#7900,#1881);
#1537=LINE('',#7903,#1882);
#1538=LINE('',#7974,#1883);
#1539=LINE('',#7984,#1884);
#1540=LINE('',#7989,#1885);
#1541=LINE('',#7997,#1886);
#1542=LINE('',#8003,#1887);
#1543=LINE('',#8011,#1888);
#1544=LINE('',#8013,#1889);
#1545=LINE('',#8015,#1890);
#1546=LINE('',#8016,#1891);
#1547=LINE('',#8019,#1892);
#1548=LINE('',#8021,#1893);
#1549=LINE('',#8022,#1894);
#1550=LINE('',#8025,#1895);
#1551=LINE('',#8027,#1896);
#1552=LINE('',#8028,#1897);
#1553=LINE('',#8031,#1898);
#1554=LINE('',#8033,#1899);
#1555=LINE('',#8034,#1900);
#1556=LINE('',#8037,#1901);
#1557=LINE('',#8039,#1902);
#1558=LINE('',#8040,#1903);
#1559=LINE('',#8042,#1904);
#1560=LINE('',#8043,#1905);
#1561=LINE('',#8055,#1906);
#1562=LINE('',#8059,#1907);
#1563=LINE('',#8063,#1908);
#1564=LINE('',#8070,#1909);
#1565=LINE('',#8072,#1910);
#1566=LINE('',#8079,#1911);
#1567=LINE('',#8085,#1912);
#1568=LINE('',#8087,#1913);
#1569=LINE('',#8089,#1914);
#1570=LINE('',#8090,#1915);
#1571=LINE('',#8095,#1916);
#1572=LINE('',#8096,#1917);
#1573=LINE('',#8099,#1918);
#1574=LINE('',#8101,#1919);
#1575=LINE('',#8102,#1920);
#1576=LINE('',#8104,#1921);
#1577=LINE('',#8111,#1922);
#1578=LINE('',#8120,#1923);
#1579=LINE('',#8126,#1924);
#1580=LINE('',#8132,#1925);
#1581=LINE('',#8138,#1926);
#1582=LINE('',#8143,#1927);
#1583=LINE('',#8160,#1928);
#1584=LINE('',#8211,#1929);
#1585=LINE('',#8215,#1930);
#1586=LINE('',#8217,#1931);
#1587=LINE('',#8219,#1932);
#1588=LINE('',#8220,#1933);
#1589=LINE('',#8223,#1934);
#1590=LINE('',#8225,#1935);
#1591=LINE('',#8226,#1936);
#1592=LINE('',#8229,#1937);
#1593=LINE('',#8231,#1938);
#1594=LINE('',#8232,#1939);
#1595=LINE('',#8241,#1940);
#1596=LINE('',#8253,#1941);
#1597=LINE('',#8256,#1942);
#1598=LINE('',#8263,#1943);
#1599=LINE('',#8269,#1944);
#1600=LINE('',#8278,#1945);
#1601=LINE('',#8284,#1946);
#1602=LINE('',#8286,#1947);
#1603=LINE('',#8288,#1948);
#1604=LINE('',#8289,#1949);
#1605=LINE('',#8294,#1950);
#1606=LINE('',#8295,#1951);
#1607=LINE('',#8298,#1952);
#1608=LINE('',#8300,#1953);
#1609=LINE('',#8301,#1954);
#1610=LINE('',#8303,#1955);
#1611=LINE('',#8310,#1956);
#1612=LINE('',#8319,#1957);
#1613=LINE('',#8325,#1958);
#1614=LINE('',#8331,#1959);
#1615=LINE('',#8337,#1960);
#1616=LINE('',#8342,#1961);
#1617=LINE('',#8359,#1962);
#1618=LINE('',#8410,#1963);
#1619=LINE('',#8414,#1964);
#1620=LINE('',#8416,#1965);
#1621=LINE('',#8418,#1966);
#1622=LINE('',#8419,#1967);
#1623=LINE('',#8423,#1968);
#1624=LINE('',#8425,#1969);
#1625=LINE('',#8427,#1970);
#1626=LINE('',#8428,#1971);
#1627=LINE('',#8430,#1972);
#1628=LINE('',#8431,#1973);
#1629=LINE('',#8441,#1974);
#1630=LINE('',#8449,#1975);
#1631=LINE('',#8454,#1976);
#1632=LINE('',#8462,#1977);
#1633=LINE('',#8468,#1978);
#1634=LINE('',#8477,#1979);
#1635=LINE('',#8483,#1980);
#1636=LINE('',#8491,#1981);
#1637=LINE('',#8512,#1982);
#1638=LINE('',#8567,#1983);
#1639=LINE('',#8572,#1984);
#1640=LINE('',#8578,#1985);
#1641=LINE('',#8586,#1986);
#1642=LINE('',#8607,#1987);
#1643=LINE('',#8662,#1988);
#1644=LINE('',#8667,#1989);
#1645=LINE('',#8673,#1990);
#1646=LINE('',#8681,#1991);
#1647=LINE('',#8683,#1992);
#1648=LINE('',#8685,#1993);
#1649=LINE('',#8687,#1994);
#1650=LINE('',#8689,#1995);
#1651=LINE('',#8691,#1996);
#1652=LINE('',#8693,#1997);
#1653=LINE('',#8694,#1998);
#1654=LINE('',#8697,#1999);
#1655=LINE('',#8699,#2000);
#1656=LINE('',#8700,#2001);
#1657=LINE('',#8703,#2002);
#1658=LINE('',#8704,#2003);
#1659=LINE('',#8707,#2004);
#1660=LINE('',#8708,#2005);
#1661=LINE('',#8711,#2006);
#1662=LINE('',#8712,#2007);
#1663=LINE('',#8716,#2008);
#1664=LINE('',#8717,#2009);
#1665=LINE('',#8719,#2010);
#1666=LINE('',#8720,#2011);
#1667=LINE('',#8722,#2012);
#1668=LINE('',#8724,#2013);
#1669=LINE('',#8726,#2014);
#1670=LINE('',#8735,#2015);
#1671=LINE('',#8739,#2016);
#1672=LINE('',#8743,#2017);
#1673=LINE('',#8750,#2018);
#1674=LINE('',#8754,#2019);
#1675=LINE('',#8758,#2020);
#1676=LINE('',#8763,#2021);
#1677=LINE('',#8765,#2022);
#1678=LINE('',#8767,#2023);
#1679=LINE('',#8768,#2024);
#1680=LINE('',#8771,#2025);
#1681=LINE('',#8773,#2026);
#1682=LINE('',#8774,#2027);
#1683=LINE('',#8777,#2028);
#1684=LINE('',#8779,#2029);
#1685=LINE('',#8780,#2030);
#1686=LINE('',#8783,#2031);
#1687=LINE('',#8785,#2032);
#1688=LINE('',#8786,#2033);
#1689=LINE('',#8789,#2034);
#1690=LINE('',#8791,#2035);
#1691=LINE('',#8792,#2036);
#1692=LINE('',#8794,#2037);
#1693=LINE('',#8795,#2038);
#1694=LINE('',#8805,#2039);
#1695=LINE('',#8809,#2040);
#1696=LINE('',#8813,#2041);
#1697=LINE('',#8820,#2042);
#1698=LINE('',#8824,#2043);
#1699=LINE('',#8828,#2044);
#1700=LINE('',#8833,#2045);
#1701=LINE('',#8835,#2046);
#1702=LINE('',#8837,#2047);
#1703=LINE('',#8838,#2048);
#1704=LINE('',#8841,#2049);
#1705=LINE('',#8843,#2050);
#1706=LINE('',#8844,#2051);
#1707=LINE('',#8847,#2052);
#1708=LINE('',#8849,#2053);
#1709=LINE('',#8850,#2054);
#1710=LINE('',#8853,#2055);
#1711=LINE('',#8855,#2056);
#1712=LINE('',#8856,#2057);
#1713=LINE('',#8859,#2058);
#1714=LINE('',#8861,#2059);
#1715=LINE('',#8862,#2060);
#1716=LINE('',#8864,#2061);
#1717=LINE('',#8865,#2062);
#1718=LINE('',#8873,#2063);
#1719=LINE('',#8879,#2064);
#1720=LINE('',#8922,#2065);
#1721=LINE('',#8943,#2066);
#1722=LINE('',#8968,#2067);
#1723=LINE('',#8969,#2068);
#1724=LINE('',#8971,#2069);
#1725=LINE('',#8973,#2070);
#1726=LINE('',#8978,#2071);
#1727=LINE('',#8981,#2072);
#1728=LINE('',#8983,#2073);
#1729=LINE('',#8991,#2074);
#1730=LINE('',#8993,#2075);
#1731=LINE('',#8995,#2076);
#1732=LINE('',#8996,#2077);
#1733=LINE('',#8999,#2078);
#1734=LINE('',#9001,#2079);
#1735=LINE('',#9002,#2080);
#1736=LINE('',#9005,#2081);
#1737=LINE('',#9007,#2082);
#1738=LINE('',#9008,#2083);
#1739=LINE('',#9011,#2084);
#1740=LINE('',#9013,#2085);
#1741=LINE('',#9014,#2086);
#1742=LINE('',#9017,#2087);
#1743=LINE('',#9019,#2088);
#1744=LINE('',#9020,#2089);
#1745=LINE('',#9022,#2090);
#1746=LINE('',#9023,#2091);
#1747=LINE('',#9031,#2092);
#1748=LINE('',#9035,#2093);
#1749=LINE('',#9039,#2094);
#1750=VECTOR('',#5652,0.25);
#1751=VECTOR('',#5659,0.25);
#1752=VECTOR('',#5666,0.25);
#1753=VECTOR('',#5673,0.25);
#1754=VECTOR('',#5678,1.);
#1755=VECTOR('',#5679,1.);
#1756=VECTOR('',#5680,1.);
#1757=VECTOR('',#5681,1.);
#1758=VECTOR('',#5684,1.);
#1759=VECTOR('',#5685,1.);
#1760=VECTOR('',#5686,1.);
#1761=VECTOR('',#5689,1.);
#1762=VECTOR('',#5690,1.);
#1763=VECTOR('',#5691,1.);
#1764=VECTOR('',#5694,1.);
#1765=VECTOR('',#5695,1.);
#1766=VECTOR('',#5704,1.);
#1767=VECTOR('',#5705,1.);
#1768=VECTOR('',#5706,1.);
#1769=VECTOR('',#5707,1.);
#1770=VECTOR('',#5710,1.);
#1771=VECTOR('',#5711,1.);
#1772=VECTOR('',#5712,1.);
#1773=VECTOR('',#5715,1.);
#1774=VECTOR('',#5716,1.);
#1775=VECTOR('',#5717,1.);
#1776=VECTOR('',#5720,1.);
#1777=VECTOR('',#5721,1.);
#1778=VECTOR('',#5730,1.);
#1779=VECTOR('',#5731,1.);
#1780=VECTOR('',#5732,1.);
#1781=VECTOR('',#5733,1.);
#1782=VECTOR('',#5736,1.);
#1783=VECTOR('',#5737,1.);
#1784=VECTOR('',#5738,1.);
#1785=VECTOR('',#5741,1.);
#1786=VECTOR('',#5742,1.);
#1787=VECTOR('',#5743,1.);
#1788=VECTOR('',#5746,1.);
#1789=VECTOR('',#5747,1.);
#1790=VECTOR('',#5758,0.34);
#1791=VECTOR('',#5765,0.34);
#1792=VECTOR('',#5772,0.33);
#1793=VECTOR('',#5779,0.33);
#1794=VECTOR('',#5784,1.);
#1795=VECTOR('',#5785,1.);
#1796=VECTOR('',#5786,1.);
#1797=VECTOR('',#5787,1.);
#1798=VECTOR('',#5790,1.);
#1799=VECTOR('',#5791,1.);
#1800=VECTOR('',#5792,1.);
#1801=VECTOR('',#5795,1.);
#1802=VECTOR('',#5796,1.);
#1803=VECTOR('',#5797,1.);
#1804=VECTOR('',#5800,1.);
#1805=VECTOR('',#5801,1.);
#1806=VECTOR('',#5812,0.425);
#1807=VECTOR('',#5819,0.645);
#1808=VECTOR('',#5832,0.425);
#1809=VECTOR('',#5839,0.645);
#1810=VECTOR('',#5852,0.34);
#1811=VECTOR('',#5859,0.34);
#1812=VECTOR('',#5866,0.33);
#1813=VECTOR('',#5873,0.33);
#1814=VECTOR('',#5878,1.);
#1815=VECTOR('',#5879,1.);
#1816=VECTOR('',#5880,1.);
#1817=VECTOR('',#5881,1.);
#1818=VECTOR('',#5884,1.);
#1819=VECTOR('',#5885,1.);
#1820=VECTOR('',#5886,1.);
#1821=VECTOR('',#5889,1.);
#1822=VECTOR('',#5890,1.);
#1823=VECTOR('',#5891,1.);
#1824=VECTOR('',#5894,1.);
#1825=VECTOR('',#5895,1.);
#1826=VECTOR('',#5906,0.425);
#1827=VECTOR('',#5913,0.645);
#1828=VECTOR('',#5926,0.425);
#1829=VECTOR('',#5933,0.645);
#1830=VECTOR('',#5948,2.05);
#1831=VECTOR('',#5955,2.05);
#1832=VECTOR('',#5964,1.);
#1833=VECTOR('',#5965,1.);
#1834=VECTOR('',#5970,1.);
#1835=VECTOR('',#5973,1.);
#1836=VECTOR('',#5976,1.);
#1837=VECTOR('',#5979,1.);
#1838=VECTOR('',#5982,1.);
#1839=VECTOR('',#5983,1.);
#1840=VECTOR('',#5986,1.);
#1841=VECTOR('',#5987,1.);
#1842=VECTOR('',#5992,1.);
#1843=VECTOR('',#5993,1.);
#1844=VECTOR('',#5996,1.);
#1845=VECTOR('',#5997,1.);
#1846=VECTOR('',#5998,1.);
#1847=VECTOR('',#5999,1.);
#1848=VECTOR('',#6004,1.);
#1849=VECTOR('',#6005,1.);
#1850=VECTOR('',#6006,1.);
#1851=VECTOR('',#6007,1.);
#1852=VECTOR('',#6008,1.);
#1853=VECTOR('',#6009,1.);
#1854=VECTOR('',#6022,1.);
#1855=VECTOR('',#6023,1.);
#1856=VECTOR('',#6024,1.);
#1857=VECTOR('',#6025,1.);
#1858=VECTOR('',#6028,1.);
#1859=VECTOR('',#6029,1.);
#1860=VECTOR('',#6030,1.);
#1861=VECTOR('',#6033,1.);
#1862=VECTOR('',#6034,1.);
#1863=VECTOR('',#6035,1.);
#1864=VECTOR('',#6038,1.);
#1865=VECTOR('',#6039,1.);
#1866=VECTOR('',#6046,0.65);
#1867=VECTOR('',#6051,0.65);
#1868=VECTOR('',#6054,1.);
#1869=VECTOR('',#6055,1.);
#1870=VECTOR('',#6056,1.);
#1871=VECTOR('',#6059,1.);
#1872=VECTOR('',#6060,1.);
#1873=VECTOR('',#6063,1.);
#1874=VECTOR('',#6064,1.);
#1875=VECTOR('',#6067,1.);
#1876=VECTOR('',#6076,1.8);
#1877=VECTOR('',#6093,0.25);
#1878=VECTOR('',#6096,0.25);
#1879=VECTOR('',#6101,1.65);
#1880=VECTOR('',#6106,0.25);
#1881=VECTOR('',#6109,0.25);
#1882=VECTOR('',#6112,0.25);
#1883=VECTOR('',#6115,0.25);
#1884=VECTOR('',#6128,1.75);
#1885=VECTOR('',#6135,1.);
#1886=VECTOR('',#6146,0.42);
#1887=VECTOR('',#6153,0.8);
#1888=VECTOR('',#6164,1.);
#1889=VECTOR('',#6165,1.);
#1890=VECTOR('',#6166,1.);
#1891=VECTOR('',#6167,1.);
#1892=VECTOR('',#6170,1.);
#1893=VECTOR('',#6171,1.);
#1894=VECTOR('',#6172,1.);
#1895=VECTOR('',#6175,1.);
#1896=VECTOR('',#6176,1.);
#1897=VECTOR('',#6177,1.);
#1898=VECTOR('',#6180,1.);
#1899=VECTOR('',#6181,1.);
#1900=VECTOR('',#6182,1.);
#1901=VECTOR('',#6185,1.);
#1902=VECTOR('',#6186,1.);
#1903=VECTOR('',#6187,1.);
#1904=VECTOR('',#6190,1.);
#1905=VECTOR('',#6191,1.);
#1906=VECTOR('',#6208,0.625);
#1907=VECTOR('',#6213,0.65);
#1908=VECTOR('',#6218,0.635);
#1909=VECTOR('',#6227,0.41);
#1910=VECTOR('',#6230,0.4);
#1911=VECTOR('',#6239,0.21);
#1912=VECTOR('',#6246,1.);
#1913=VECTOR('',#6247,1.);
#1914=VECTOR('',#6248,1.);
#1915=VECTOR('',#6249,1.);
#1916=VECTOR('',#6254,1.);
#1917=VECTOR('',#6255,1.);
#1918=VECTOR('',#6258,1.);
#1919=VECTOR('',#6259,1.);
#1920=VECTOR('',#6260,1.);
#1921=VECTOR('',#6263,1.);
#1922=VECTOR('',#6272,1.);
#1923=VECTOR('',#6285,0.33);
#1924=VECTOR('',#6292,0.33);
#1925=VECTOR('',#6299,0.33);
#1926=VECTOR('',#6306,0.33);
#1927=VECTOR('',#6311,1.);
#1928=VECTOR('',#6318,0.21);
#1929=VECTOR('',#6323,1.);
#1930=VECTOR('',#6326,1.);
#1931=VECTOR('',#6327,1.);
#1932=VECTOR('',#6328,1.);
#1933=VECTOR('',#6329,1.);
#1934=VECTOR('',#6332,1.);
#1935=VECTOR('',#6333,1.);
#1936=VECTOR('',#6334,1.);
#1937=VECTOR('',#6337,1.);
#1938=VECTOR('',#6338,1.);
#1939=VECTOR('',#6339,1.);
#1940=VECTOR('',#6350,2.);
#1941=VECTOR('',#6367,4.);
#1942=VECTOR('',#6372,1.7);
#1943=VECTOR('',#6381,0.275);
#1944=VECTOR('',#6388,1.1);
#1945=VECTOR('',#6401,0.21);
#1946=VECTOR('',#6408,1.);
#1947=VECTOR('',#6409,1.);
#1948=VECTOR('',#6410,1.);
#1949=VECTOR('',#6411,1.);
#1950=VECTOR('',#6416,1.);
#1951=VECTOR('',#6417,1.);
#1952=VECTOR('',#6420,1.);
#1953=VECTOR('',#6421,1.);
#1954=VECTOR('',#6422,1.);
#1955=VECTOR('',#6425,1.);
#1956=VECTOR('',#6434,1.);
#1957=VECTOR('',#6447,0.33);
#1958=VECTOR('',#6454,0.33);
#1959=VECTOR('',#6461,0.33);
#1960=VECTOR('',#6468,0.33);
#1961=VECTOR('',#6473,1.);
#1962=VECTOR('',#6480,0.21);
#1963=VECTOR('',#6485,1.);
#1964=VECTOR('',#6488,1.);
#1965=VECTOR('',#6489,1.);
#1966=VECTOR('',#6490,1.);
#1967=VECTOR('',#6491,1.);
#1968=VECTOR('',#6494,1.);
#1969=VECTOR('',#6495,1.);
#1970=VECTOR('',#6496,1.);
#1971=VECTOR('',#6497,1.);
#1972=VECTOR('',#6500,1.);
#1973=VECTOR('',#6501,1.);
#1974=VECTOR('',#6516,2.);
#1975=VECTOR('',#6525,4.);
#1976=VECTOR('',#6532,1.7);
#1977=VECTOR('',#6543,0.275);
#1978=VECTOR('',#6550,1.1);
#1979=VECTOR('',#6563,1.);
#1980=VECTOR('',#6570,2.);
#1981=VECTOR('',#6581,1.);
#1982=VECTOR('',#6588,0.21);
#1983=VECTOR('',#6593,1.);
#1984=VECTOR('',#6598,1.005);
#1985=VECTOR('',#6605,1.5);
#1986=VECTOR('',#6616,1.);
#1987=VECTOR('',#6623,0.21);
#1988=VECTOR('',#6628,1.);
#1989=VECTOR('',#6633,1.005);
#1990=VECTOR('',#6640,1.5);
#1991=VECTOR('',#6651,1.);
#1992=VECTOR('',#6652,1.);
#1993=VECTOR('',#6653,1.);
#1994=VECTOR('',#6654,1.);
#1995=VECTOR('',#6655,1.);
#1996=VECTOR('',#6656,1.);
#1997=VECTOR('',#6657,1.);
#1998=VECTOR('',#6658,1.);
#1999=VECTOR('',#6661,1.);
#2000=VECTOR('',#6662,1.);
#2001=VECTOR('',#6663,1.);
#2002=VECTOR('',#6666,1.);
#2003=VECTOR('',#6667,1.);
#2004=VECTOR('',#6670,1.);
#2005=VECTOR('',#6671,1.);
#2006=VECTOR('',#6674,1.);
#2007=VECTOR('',#6675,1.);
#2008=VECTOR('',#6678,1.);
#2009=VECTOR('',#6679,1.);
#2010=VECTOR('',#6680,1.);
#2011=VECTOR('',#6681,1.);
#2012=VECTOR('',#6684,1.);
#2013=VECTOR('',#6687,1.);
#2014=VECTOR('',#6690,1.);
#2015=VECTOR('',#6703,0.4);
#2016=VECTOR('',#6708,0.425);
#2017=VECTOR('',#6713,0.41);
#2018=VECTOR('',#6722,0.26);
#2019=VECTOR('',#6727,0.25);
#2020=VECTOR('',#6732,0.225);
#2021=VECTOR('',#6737,1.);
#2022=VECTOR('',#6738,1.);
#2023=VECTOR('',#6739,1.);
#2024=VECTOR('',#6740,1.);
#2025=VECTOR('',#6743,1.);
#2026=VECTOR('',#6744,1.);
#2027=VECTOR('',#6745,1.);
#2028=VECTOR('',#6748,1.);
#2029=VECTOR('',#6749,1.);
#2030=VECTOR('',#6750,1.);
#2031=VECTOR('',#6753,1.);
#2032=VECTOR('',#6754,1.);
#2033=VECTOR('',#6755,1.);
#2034=VECTOR('',#6758,1.);
#2035=VECTOR('',#6759,1.);
#2036=VECTOR('',#6760,1.);
#2037=VECTOR('',#6763,1.);
#2038=VECTOR('',#6764,1.);
#2039=VECTOR('',#6779,0.475);
#2040=VECTOR('',#6784,0.5);
#2041=VECTOR('',#6789,0.485);
#2042=VECTOR('',#6798,0.31);
#2043=VECTOR('',#6803,0.3);
#2044=VECTOR('',#6808,0.27);
#2045=VECTOR('',#6813,1.);
#2046=VECTOR('',#6814,1.);
#2047=VECTOR('',#6815,1.);
#2048=VECTOR('',#6816,1.);
#2049=VECTOR('',#6819,1.);
#2050=VECTOR('',#6820,1.);
#2051=VECTOR('',#6821,1.);
#2052=VECTOR('',#6824,1.);
#2053=VECTOR('',#6825,1.);
#2054=VECTOR('',#6826,1.);
#2055=VECTOR('',#6829,1.);
#2056=VECTOR('',#6830,1.);
#2057=VECTOR('',#6831,1.);
#2058=VECTOR('',#6834,1.);
#2059=VECTOR('',#6835,1.);
#2060=VECTOR('',#6836,1.);
#2061=VECTOR('',#6839,1.);
#2062=VECTOR('',#6840,1.);
#2063=VECTOR('',#6851,0.32);
#2064=VECTOR('',#6858,0.6);
#2065=VECTOR('',#6923,0.576175134594813);
#2066=VECTOR('',#6930,0.576175134594813);
#2067=VECTOR('',#6933,1.);
#2068=VECTOR('',#6934,1.);
#2069=VECTOR('',#6937,1.);
#2070=VECTOR('',#6940,1.);
#2071=VECTOR('',#6945,0.3);
#2072=VECTOR('',#6950,1.);
#2073=VECTOR('',#6953,1.);
#2074=VECTOR('',#6964,1.);
#2075=VECTOR('',#6965,1.);
#2076=VECTOR('',#6966,1.);
#2077=VECTOR('',#6967,1.);
#2078=VECTOR('',#6970,1.);
#2079=VECTOR('',#6971,1.);
#2080=VECTOR('',#6972,1.);
#2081=VECTOR('',#6975,1.);
#2082=VECTOR('',#6976,1.);
#2083=VECTOR('',#6977,1.);
#2084=VECTOR('',#6980,1.);
#2085=VECTOR('',#6981,1.);
#2086=VECTOR('',#6982,1.);
#2087=VECTOR('',#6985,1.);
#2088=VECTOR('',#6986,1.);
#2089=VECTOR('',#6987,1.);
#2090=VECTOR('',#6990,1.);
#2091=VECTOR('',#6991,1.);
#2092=VECTOR('',#7002,0.235);
#2093=VECTOR('',#7007,0.25);
#2094=VECTOR('',#7012,0.2125);
#2095=CIRCLE('',#5097,0.25);
#2096=CIRCLE('',#5098,0.25);
#2097=CIRCLE('',#5100,0.25);
#2098=CIRCLE('',#5101,0.25);
#2099=CIRCLE('',#5103,0.25);
#2100=CIRCLE('',#5104,0.25);
#2101=CIRCLE('',#5106,0.25);
#2102=CIRCLE('',#5107,0.25);
#2103=CIRCLE('',#5130,0.34);
#2104=CIRCLE('',#5131,0.34);
#2105=CIRCLE('',#5133,0.34);
#2106=CIRCLE('',#5134,0.34);
#2107=CIRCLE('',#5136,0.33);
#2108=CIRCLE('',#5137,0.33);
#2109=CIRCLE('',#5139,0.33);
#2110=CIRCLE('',#5140,0.33);
#2111=CIRCLE('',#5149,0.425);
#2112=CIRCLE('',#5150,0.425);
#2113=CIRCLE('',#5152,0.645);
#2114=CIRCLE('',#5153,0.645);
#2115=CIRCLE('',#5158,0.425);
#2116=CIRCLE('',#5159,0.425);
#2117=CIRCLE('',#5161,0.645);
#2118=CIRCLE('',#5162,0.645);
#2119=CIRCLE('',#5167,0.34);
#2120=CIRCLE('',#5168,0.34);
#2121=CIRCLE('',#5170,0.34);
#2122=CIRCLE('',#5171,0.34);
#2123=CIRCLE('',#5173,0.33);
#2124=CIRCLE('',#5174,0.33);
#2125=CIRCLE('',#5176,0.33);
#2126=CIRCLE('',#5177,0.33);
#2127=CIRCLE('',#5186,0.425);
#2128=CIRCLE('',#5187,0.425);
#2129=CIRCLE('',#5189,0.645);
#2130=CIRCLE('',#5190,0.645);
#2131=CIRCLE('',#5195,0.425);
#2132=CIRCLE('',#5196,0.425);
#2133=CIRCLE('',#5198,0.645);
#2134=CIRCLE('',#5199,0.645);
#2135=CIRCLE('',#5205,2.05);
#2136=CIRCLE('',#5206,2.05);
#2137=CIRCLE('',#5208,2.05);
#2138=CIRCLE('',#5209,2.05);
#2139=CIRCLE('',#5211,2.35);
#2140=CIRCLE('',#5213,2.8);
#2141=CIRCLE('',#5215,2.8);
#2142=CIRCLE('',#5217,2.8);
#2143=CIRCLE('',#5220,2.8);
#2144=CIRCLE('',#5223,0.65);
#2145=CIRCLE('',#5224,0.65);
#2146=CIRCLE('',#5226,2.8);
#2147=CIRCLE('',#5227,2.8);
#2148=CIRCLE('',#5236,0.65);
#2149=CIRCLE('',#5238,0.65);
#2150=CIRCLE('',#5246,1.8);
#2151=CIRCLE('',#5247,1.8);
#2152=CIRCLE('',#5249,2.19089023002066);
#2153=CIRCLE('',#5251,2.35);
#2154=CIRCLE('',#5252,2.19089023002066);
#2155=CIRCLE('',#5257,1.65);
#2156=CIRCLE('',#5258,1.65);
#2157=CIRCLE('',#5264,1.);
#2158=CIRCLE('',#5266,1.75);
#2159=CIRCLE('',#5268,1.75);
#2160=CIRCLE('',#5270,1.);
#2161=CIRCLE('',#5276,0.42);
#2162=CIRCLE('',#5277,0.42);
#2163=CIRCLE('',#5279,0.8);
#2164=CIRCLE('',#5280,0.8);
#2165=CIRCLE('',#5293,0.3933);
#2166=CIRCLE('',#5295,0.6);
#2167=CIRCLE('',#5297,0.65);
#2168=CIRCLE('',#5299,0.65);
#2169=CIRCLE('',#5301,0.62);
#2170=CIRCLE('',#5303,0.42);
#2171=CIRCLE('',#5305,0.3933);
#2172=CIRCLE('',#5310,0.21);
#2173=CIRCLE('',#5311,0.21);
#2174=CIRCLE('',#5315,1.);
#2175=CIRCLE('',#5319,1.);
#2176=CIRCLE('',#5321,1.);
#2177=CIRCLE('',#5322,1.);
#2178=CIRCLE('',#5327,0.33);
#2179=CIRCLE('',#5328,0.33);
#2180=CIRCLE('',#5330,0.33);
#2181=CIRCLE('',#5331,0.33);
#2182=CIRCLE('',#5333,0.33);
#2183=CIRCLE('',#5334,0.33);
#2184=CIRCLE('',#5336,0.33);
#2185=CIRCLE('',#5337,0.33);
#2186=CIRCLE('',#5339,0.21);
#2187=CIRCLE('',#5341,0.21);
#2188=CIRCLE('',#5342,0.21);
#2189=CIRCLE('',#5348,1.7);
#2190=CIRCLE('',#5349,1.);
#2191=CIRCLE('',#5351,2.);
#2192=CIRCLE('',#5352,2.);
#2193=CIRCLE('',#5354,1.);
#2194=CIRCLE('',#5356,4.);
#2195=CIRCLE('',#5357,1.7);
#2196=CIRCLE('',#5359,4.);
#2197=CIRCLE('',#5365,0.275);
#2198=CIRCLE('',#5366,0.275);
#2199=CIRCLE('',#5368,1.1);
#2200=CIRCLE('',#5369,1.1);
#2201=CIRCLE('',#5374,0.21);
#2202=CIRCLE('',#5375,0.21);
#2203=CIRCLE('',#5379,1.);
#2204=CIRCLE('',#5383,1.);
#2205=CIRCLE('',#5385,1.);
#2206=CIRCLE('',#5386,1.);
#2207=CIRCLE('',#5391,0.33);
#2208=CIRCLE('',#5392,0.33);
#2209=CIRCLE('',#5394,0.33);
#2210=CIRCLE('',#5395,0.33);
#2211=CIRCLE('',#5397,0.33);
#2212=CIRCLE('',#5398,0.33);
#2213=CIRCLE('',#5400,0.33);
#2214=CIRCLE('',#5401,0.33);
#2215=CIRCLE('',#5403,0.21);
#2216=CIRCLE('',#5405,0.21);
#2217=CIRCLE('',#5406,0.21);
#2218=CIRCLE('',#5412,2.);
#2219=CIRCLE('',#5413,1.);
#2220=CIRCLE('',#5415,1.);
#2221=CIRCLE('',#5417,2.);
#2222=CIRCLE('',#5419,4.);
#2223=CIRCLE('',#5420,1.7);
#2224=CIRCLE('',#5422,4.);
#2225=CIRCLE('',#5424,1.7);
#2226=CIRCLE('',#5429,0.275);
#2227=CIRCLE('',#5430,0.275);
#2228=CIRCLE('',#5432,1.1);
#2229=CIRCLE('',#5433,1.1);
#2230=CIRCLE('',#5438,1.);
#2231=CIRCLE('',#5439,1.);
#2232=CIRCLE('',#5441,2.);
#2233=CIRCLE('',#5442,2.);
#2234=CIRCLE('',#5447,0.21);
#2235=CIRCLE('',#5449,0.21);
#2236=CIRCLE('',#5450,0.21);
#2237=CIRCLE('',#5453,1.005);
#2238=CIRCLE('',#5454,1.005);
#2239=CIRCLE('',#5456,1.5);
#2240=CIRCLE('',#5457,1.5);
#2241=CIRCLE('',#5462,0.21);
#2242=CIRCLE('',#5464,0.21);
#2243=CIRCLE('',#5465,0.21);
#2244=CIRCLE('',#5468,1.005);
#2245=CIRCLE('',#5469,1.005);
#2246=CIRCLE('',#5471,1.5);
#2247=CIRCLE('',#5472,1.5);
#2248=CIRCLE('',#5488,0.375);
#2249=CIRCLE('',#5490,0.425);
#2250=CIRCLE('',#5492,0.425);
#2251=CIRCLE('',#5494,0.395);
#2252=CIRCLE('',#5496,0.27);
#2253=CIRCLE('',#5498,0.24505);
#2254=CIRCLE('',#5500,0.24505);
#2255=CIRCLE('',#5502,0.2);
#2256=CIRCLE('',#5514,0.45);
#2257=CIRCLE('',#5516,0.5);
#2258=CIRCLE('',#5518,0.5);
#2259=CIRCLE('',#5520,0.47);
#2260=CIRCLE('',#5522,0.32);
#2261=CIRCLE('',#5524,0.2942);
#2262=CIRCLE('',#5526,0.2942);
#2263=CIRCLE('',#5528,0.24);
#2264=CIRCLE('',#5540,0.32);
#2265=CIRCLE('',#5541,0.32);
#2266=CIRCLE('',#5543,0.6);
#2267=CIRCLE('',#5544,0.6);
#2268=CIRCLE('',#5576,0.475);
#2269=CIRCLE('',#5578,0.475);
#2270=CIRCLE('',#5583,0.25175);
#2271=CIRCLE('',#5584,0.25175);
#2272=CIRCLE('',#5599,0.22);
#2273=CIRCLE('',#5601,0.24505);
#2274=CIRCLE('',#5603,0.24505);
#2275=CIRCLE('',#5605,0.175);
#2276=VERTEX_POINT('',#7089);
#2277=VERTEX_POINT('',#7091);
#2278=VERTEX_POINT('',#7095);
#2279=VERTEX_POINT('',#7097);
#2280=VERTEX_POINT('',#7101);
#2281=VERTEX_POINT('',#7103);
#2282=VERTEX_POINT('',#7107);
#2283=VERTEX_POINT('',#7109);
#2284=VERTEX_POINT('',#7113);
#2285=VERTEX_POINT('',#7114);
#2286=VERTEX_POINT('',#7116);
#2287=VERTEX_POINT('',#7118);
#2288=VERTEX_POINT('',#7122);
#2289=VERTEX_POINT('',#7124);
#2290=VERTEX_POINT('',#7128);
#2291=VERTEX_POINT('',#7130);
#2292=VERTEX_POINT('',#7140);
#2293=VERTEX_POINT('',#7141);
#2294=VERTEX_POINT('',#7143);
#2295=VERTEX_POINT('',#7145);
#2296=VERTEX_POINT('',#7149);
#2297=VERTEX_POINT('',#7151);
#2298=VERTEX_POINT('',#7155);
#2299=VERTEX_POINT('',#7157);
#2300=VERTEX_POINT('',#7167);
#2301=VERTEX_POINT('',#7168);
#2302=VERTEX_POINT('',#7170);
#2303=VERTEX_POINT('',#7172);
#2304=VERTEX_POINT('',#7176);
#2305=VERTEX_POINT('',#7178);
#2306=VERTEX_POINT('',#7182);
#2307=VERTEX_POINT('',#7184);
#2308=VERTEX_POINT('',#7194);
#2309=VERTEX_POINT('',#7196);
#2310=VERTEX_POINT('',#7200);
#2311=VERTEX_POINT('',#7202);
#2312=VERTEX_POINT('',#7206);
#2313=VERTEX_POINT('',#7208);
#2314=VERTEX_POINT('',#7212);
#2315=VERTEX_POINT('',#7214);
#2316=VERTEX_POINT('',#7218);
#2317=VERTEX_POINT('',#7219);
#2318=VERTEX_POINT('',#7221);
#2319=VERTEX_POINT('',#7223);
#2320=VERTEX_POINT('',#7227);
#2321=VERTEX_POINT('',#7229);
#2322=VERTEX_POINT('',#7233);
#2323=VERTEX_POINT('',#7235);
#2324=VERTEX_POINT('',#7245);
#2325=VERTEX_POINT('',#7247);
#2326=VERTEX_POINT('',#7251);
#2327=VERTEX_POINT('',#7253);
#2328=VERTEX_POINT('',#7260);
#2329=VERTEX_POINT('',#7262);
#2330=VERTEX_POINT('',#7266);
#2331=VERTEX_POINT('',#7268);
#2332=VERTEX_POINT('',#7275);
#2333=VERTEX_POINT('',#7277);
#2334=VERTEX_POINT('',#7281);
#2335=VERTEX_POINT('',#7283);
#2336=VERTEX_POINT('',#7287);
#2337=VERTEX_POINT('',#7289);
#2338=VERTEX_POINT('',#7293);
#2339=VERTEX_POINT('',#7295);
#2340=VERTEX_POINT('',#7299);
#2341=VERTEX_POINT('',#7300);
#2342=VERTEX_POINT('',#7302);
#2343=VERTEX_POINT('',#7304);
#2344=VERTEX_POINT('',#7308);
#2345=VERTEX_POINT('',#7310);
#2346=VERTEX_POINT('',#7314);
#2347=VERTEX_POINT('',#7316);
#2348=VERTEX_POINT('',#7326);
#2349=VERTEX_POINT('',#7328);
#2350=VERTEX_POINT('',#7332);
#2351=VERTEX_POINT('',#7334);
#2352=VERTEX_POINT('',#7341);
#2353=VERTEX_POINT('',#7343);
#2354=VERTEX_POINT('',#7347);
#2355=VERTEX_POINT('',#7349);
#2356=VERTEX_POINT('',#7357);
#2357=VERTEX_POINT('',#7359);
#2358=VERTEX_POINT('',#7363);
#2359=VERTEX_POINT('',#7365);
#2360=VERTEX_POINT('',#7369);
#2361=VERTEX_POINT('',#7370);
#2362=VERTEX_POINT('',#7373);
#2363=VERTEX_POINT('',#7374);
#2364=VERTEX_POINT('',#7376);
#2365=VERTEX_POINT('',#7380);
#2366=VERTEX_POINT('',#7381);
#2367=VERTEX_POINT('',#7383);
#2368=VERTEX_POINT('',#7387);
#2369=VERTEX_POINT('',#7388);
#2370=VERTEX_POINT('',#7390);
#2371=VERTEX_POINT('',#7397);
#2372=VERTEX_POINT('',#7398);
#2373=VERTEX_POINT('',#7400);
#2374=VERTEX_POINT('',#7407);
#2375=VERTEX_POINT('',#7408);
#2376=VERTEX_POINT('',#7410);
#2377=VERTEX_POINT('',#7412);
#2378=VERTEX_POINT('',#7415);
#2379=VERTEX_POINT('',#7417);
#2380=VERTEX_POINT('',#7419);
#2381=VERTEX_POINT('',#7421);
#2382=VERTEX_POINT('',#7424);
#2383=VERTEX_POINT('',#7426);
#2384=VERTEX_POINT('',#7435);
#2385=VERTEX_POINT('',#7436);
#2386=VERTEX_POINT('',#7438);
#2387=VERTEX_POINT('',#7440);
#2388=VERTEX_POINT('',#7444);
#2389=VERTEX_POINT('',#7446);
#2390=VERTEX_POINT('',#7450);
#2391=VERTEX_POINT('',#7452);
#2392=VERTEX_POINT('',#7460);
#2393=VERTEX_POINT('',#7464);
#2394=VERTEX_POINT('',#7468);
#2395=VERTEX_POINT('',#7469);
#2396=VERTEX_POINT('',#7474);
#2397=VERTEX_POINT('',#7478);
#2398=VERTEX_POINT('',#7486);
#2399=VERTEX_POINT('',#7488);
#2400=VERTEX_POINT('',#7492);
#2401=VERTEX_POINT('',#7495);
#2402=VERTEX_POINT('',#7496);
#2403=VERTEX_POINT('',#7498);
#2404=VERTEX_POINT('',#7502);
#2405=VERTEX_POINT('',#7503);
#2406=VERTEX_POINT('',#7514);
#2407=VERTEX_POINT('',#7543);
#2408=VERTEX_POINT('',#7580);
#2409=VERTEX_POINT('',#7615);
#2410=VERTEX_POINT('',#7617);
#2411=VERTEX_POINT('',#7628);
#2412=VERTEX_POINT('',#7658);
#2413=VERTEX_POINT('',#7660);
#2414=VERTEX_POINT('',#7663);
#2415=VERTEX_POINT('',#7664);
#2416=VERTEX_POINT('',#7683);
#2417=VERTEX_POINT('',#7704);
#2418=VERTEX_POINT('',#7705);
#2419=VERTEX_POINT('',#7724);
#2420=VERTEX_POINT('',#7745);
#2421=VERTEX_POINT('',#7746);
#2422=VERTEX_POINT('',#7765);
#2423=VERTEX_POINT('',#7786);
#2424=VERTEX_POINT('',#7787);
#2425=VERTEX_POINT('',#7806);
#2426=VERTEX_POINT('',#7828);
#2427=VERTEX_POINT('',#7865);
#2428=VERTEX_POINT('',#7902);
#2429=VERTEX_POINT('',#7939);
#2430=VERTEX_POINT('',#7976);
#2431=VERTEX_POINT('',#7979);
#2432=VERTEX_POINT('',#7982);
#2433=VERTEX_POINT('',#7986);
#2434=VERTEX_POINT('',#7994);
#2435=VERTEX_POINT('',#7996);
#2436=VERTEX_POINT('',#8000);
#2437=VERTEX_POINT('',#8002);
#2438=VERTEX_POINT('',#8009);
#2439=VERTEX_POINT('',#8010);
#2440=VERTEX_POINT('',#8012);
#2441=VERTEX_POINT('',#8014);
#2442=VERTEX_POINT('',#8018);
#2443=VERTEX_POINT('',#8020);
#2444=VERTEX_POINT('',#8024);
#2445=VERTEX_POINT('',#8026);
#2446=VERTEX_POINT('',#8030);
#2447=VERTEX_POINT('',#8032);
#2448=VERTEX_POINT('',#8036);
#2449=VERTEX_POINT('',#8038);
#2450=VERTEX_POINT('',#8047);
#2451=VERTEX_POINT('',#8050);
#2452=VERTEX_POINT('',#8053);
#2453=VERTEX_POINT('',#8057);
#2454=VERTEX_POINT('',#8061);
#2455=VERTEX_POINT('',#8065);
#2456=VERTEX_POINT('',#8068);
#2457=VERTEX_POINT('',#8076);
#2458=VERTEX_POINT('',#8078);
#2459=VERTEX_POINT('',#8083);
#2460=VERTEX_POINT('',#8084);
#2461=VERTEX_POINT('',#8086);
#2462=VERTEX_POINT('',#8088);
#2463=VERTEX_POINT('',#8092);
#2464=VERTEX_POINT('',#8094);
#2465=VERTEX_POINT('',#8098);
#2466=VERTEX_POINT('',#8100);
#2467=VERTEX_POINT('',#8108);
#2468=VERTEX_POINT('',#8110);
#2469=VERTEX_POINT('',#8117);
#2470=VERTEX_POINT('',#8119);
#2471=VERTEX_POINT('',#8123);
#2472=VERTEX_POINT('',#8125);
#2473=VERTEX_POINT('',#8129);
#2474=VERTEX_POINT('',#8131);
#2475=VERTEX_POINT('',#8135);
#2476=VERTEX_POINT('',#8137);
#2477=VERTEX_POINT('',#8141);
#2478=VERTEX_POINT('',#8142);
#2479=VERTEX_POINT('',#8146);
#2480=VERTEX_POINT('',#8157);
#2481=VERTEX_POINT('',#8159);
#2482=VERTEX_POINT('',#8161);
#2483=VERTEX_POINT('',#8198);
#2484=VERTEX_POINT('',#8213);
#2485=VERTEX_POINT('',#8214);
#2486=VERTEX_POINT('',#8216);
#2487=VERTEX_POINT('',#8218);
#2488=VERTEX_POINT('',#8222);
#2489=VERTEX_POINT('',#8224);
#2490=VERTEX_POINT('',#8228);
#2491=VERTEX_POINT('',#8230);
#2492=VERTEX_POINT('',#8234);
#2493=VERTEX_POINT('',#8238);
#2494=VERTEX_POINT('',#8240);
#2495=VERTEX_POINT('',#8246);
#2496=VERTEX_POINT('',#8248);
#2497=VERTEX_POINT('',#8251);
#2498=VERTEX_POINT('',#8260);
#2499=VERTEX_POINT('',#8262);
#2500=VERTEX_POINT('',#8266);
#2501=VERTEX_POINT('',#8268);
#2502=VERTEX_POINT('',#8275);
#2503=VERTEX_POINT('',#8277);
#2504=VERTEX_POINT('',#8282);
#2505=VERTEX_POINT('',#8283);
#2506=VERTEX_POINT('',#8285);
#2507=VERTEX_POINT('',#8287);
#2508=VERTEX_POINT('',#8291);
#2509=VERTEX_POINT('',#8293);
#2510=VERTEX_POINT('',#8297);
#2511=VERTEX_POINT('',#8299);
#2512=VERTEX_POINT('',#8307);
#2513=VERTEX_POINT('',#8309);
#2514=VERTEX_POINT('',#8316);
#2515=VERTEX_POINT('',#8318);
#2516=VERTEX_POINT('',#8322);
#2517=VERTEX_POINT('',#8324);
#2518=VERTEX_POINT('',#8328);
#2519=VERTEX_POINT('',#8330);
#2520=VERTEX_POINT('',#8334);
#2521=VERTEX_POINT('',#8336);
#2522=VERTEX_POINT('',#8340);
#2523=VERTEX_POINT('',#8341);
#2524=VERTEX_POINT('',#8345);
#2525=VERTEX_POINT('',#8356);
#2526=VERTEX_POINT('',#8358);
#2527=VERTEX_POINT('',#8360);
#2528=VERTEX_POINT('',#8397);
#2529=VERTEX_POINT('',#8412);
#2530=VERTEX_POINT('',#8413);
#2531=VERTEX_POINT('',#8415);
#2532=VERTEX_POINT('',#8417);
#2533=VERTEX_POINT('',#8421);
#2534=VERTEX_POINT('',#8422);
#2535=VERTEX_POINT('',#8424);
#2536=VERTEX_POINT('',#8426);
#2537=VERTEX_POINT('',#8433);
#2538=VERTEX_POINT('',#8439);
#2539=VERTEX_POINT('',#8443);
#2540=VERTEX_POINT('',#8445);
#2541=VERTEX_POINT('',#8448);
#2542=VERTEX_POINT('',#8452);
#2543=VERTEX_POINT('',#8459);
#2544=VERTEX_POINT('',#8461);
#2545=VERTEX_POINT('',#8465);
#2546=VERTEX_POINT('',#8467);
#2547=VERTEX_POINT('',#8474);
#2548=VERTEX_POINT('',#8476);
#2549=VERTEX_POINT('',#8480);
#2550=VERTEX_POINT('',#8482);
#2551=VERTEX_POINT('',#8489);
#2552=VERTEX_POINT('',#8490);
#2553=VERTEX_POINT('',#8494);
#2554=VERTEX_POINT('',#8509);
#2555=VERTEX_POINT('',#8511);
#2556=VERTEX_POINT('',#8513);
#2557=VERTEX_POINT('',#8550);
#2558=VERTEX_POINT('',#8569);
#2559=VERTEX_POINT('',#8571);
#2560=VERTEX_POINT('',#8575);
#2561=VERTEX_POINT('',#8577);
#2562=VERTEX_POINT('',#8584);
#2563=VERTEX_POINT('',#8585);
#2564=VERTEX_POINT('',#8589);
#2565=VERTEX_POINT('',#8604);
#2566=VERTEX_POINT('',#8606);
#2567=VERTEX_POINT('',#8608);
#2568=VERTEX_POINT('',#8645);
#2569=VERTEX_POINT('',#8664);
#2570=VERTEX_POINT('',#8666);
#2571=VERTEX_POINT('',#8670);
#2572=VERTEX_POINT('',#8672);
#2573=VERTEX_POINT('',#8679);
#2574=VERTEX_POINT('',#8680);
#2575=VERTEX_POINT('',#8682);
#2576=VERTEX_POINT('',#8684);
#2577=VERTEX_POINT('',#8686);
#2578=VERTEX_POINT('',#8688);
#2579=VERTEX_POINT('',#8690);
#2580=VERTEX_POINT('',#8692);
#2581=VERTEX_POINT('',#8696);
#2582=VERTEX_POINT('',#8698);
#2583=VERTEX_POINT('',#8702);
#2584=VERTEX_POINT('',#8706);
#2585=VERTEX_POINT('',#8710);
#2586=VERTEX_POINT('',#8714);
#2587=VERTEX_POINT('',#8715);
#2588=VERTEX_POINT('',#8718);
#2589=VERTEX_POINT('',#8730);
#2590=VERTEX_POINT('',#8733);
#2591=VERTEX_POINT('',#8737);
#2592=VERTEX_POINT('',#8741);
#2593=VERTEX_POINT('',#8745);
#2594=VERTEX_POINT('',#8748);
#2595=VERTEX_POINT('',#8752);
#2596=VERTEX_POINT('',#8756);
#2597=VERTEX_POINT('',#8761);
#2598=VERTEX_POINT('',#8762);
#2599=VERTEX_POINT('',#8764);
#2600=VERTEX_POINT('',#8766);
#2601=VERTEX_POINT('',#8770);
#2602=VERTEX_POINT('',#8772);
#2603=VERTEX_POINT('',#8776);
#2604=VERTEX_POINT('',#8778);
#2605=VERTEX_POINT('',#8782);
#2606=VERTEX_POINT('',#8784);
#2607=VERTEX_POINT('',#8788);
#2608=VERTEX_POINT('',#8790);
#2609=VERTEX_POINT('',#8800);
#2610=VERTEX_POINT('',#8803);
#2611=VERTEX_POINT('',#8807);
#2612=VERTEX_POINT('',#8811);
#2613=VERTEX_POINT('',#8815);
#2614=VERTEX_POINT('',#8818);
#2615=VERTEX_POINT('',#8822);
#2616=VERTEX_POINT('',#8826);
#2617=VERTEX_POINT('',#8831);
#2618=VERTEX_POINT('',#8832);
#2619=VERTEX_POINT('',#8834);
#2620=VERTEX_POINT('',#8836);
#2621=VERTEX_POINT('',#8840);
#2622=VERTEX_POINT('',#8842);
#2623=VERTEX_POINT('',#8846);
#2624=VERTEX_POINT('',#8848);
#2625=VERTEX_POINT('',#8852);
#2626=VERTEX_POINT('',#8854);
#2627=VERTEX_POINT('',#8858);
#2628=VERTEX_POINT('',#8860);
#2629=VERTEX_POINT('',#8870);
#2630=VERTEX_POINT('',#8872);
#2631=VERTEX_POINT('',#8876);
#2632=VERTEX_POINT('',#8878);
#2633=VERTEX_POINT('',#8912);
#2634=VERTEX_POINT('',#8913);
#2635=VERTEX_POINT('',#8917);
#2636=VERTEX_POINT('',#8921);
#2637=VERTEX_POINT('',#8924);
#2638=VERTEX_POINT('',#8928);
#2639=VERTEX_POINT('',#8932);
#2640=VERTEX_POINT('',#8940);
#2641=VERTEX_POINT('',#8942);
#2642=VERTEX_POINT('',#8944);
#2643=VERTEX_POINT('',#8948);
#2644=VERTEX_POINT('',#8952);
#2645=VERTEX_POINT('',#8956);
#2646=VERTEX_POINT('',#8960);
#2647=VERTEX_POINT('',#8975);
#2648=VERTEX_POINT('',#8977);
#2649=VERTEX_POINT('',#8989);
#2650=VERTEX_POINT('',#8990);
#2651=VERTEX_POINT('',#8992);
#2652=VERTEX_POINT('',#8994);
#2653=VERTEX_POINT('',#8998);
#2654=VERTEX_POINT('',#9000);
#2655=VERTEX_POINT('',#9004);
#2656=VERTEX_POINT('',#9006);
#2657=VERTEX_POINT('',#9010);
#2658=VERTEX_POINT('',#9012);
#2659=VERTEX_POINT('',#9016);
#2660=VERTEX_POINT('',#9018);
#2661=VERTEX_POINT('',#9026);
#2662=VERTEX_POINT('',#9029);
#2663=VERTEX_POINT('',#9033);
#2664=VERTEX_POINT('',#9037);
#2665=EDGE_CURVE('',#2276,#2276,#2095,.T.);
#2666=EDGE_CURVE('',#2276,#2277,#1405,.T.);
#2667=EDGE_CURVE('',#2277,#2277,#2096,.T.);
#2668=EDGE_CURVE('',#2278,#2278,#2097,.T.);
#2669=EDGE_CURVE('',#2278,#2279,#1406,.T.);
#2670=EDGE_CURVE('',#2279,#2279,#2098,.T.);
#2671=EDGE_CURVE('',#2280,#2280,#2099,.T.);
#2672=EDGE_CURVE('',#2280,#2281,#1407,.T.);
#2673=EDGE_CURVE('',#2281,#2281,#2100,.T.);
#2674=EDGE_CURVE('',#2282,#2282,#2101,.T.);
#2675=EDGE_CURVE('',#2282,#2283,#1408,.T.);
#2676=EDGE_CURVE('',#2283,#2283,#2102,.T.);
#2677=EDGE_CURVE('',#2284,#2285,#1409,.T.);
#2678=EDGE_CURVE('',#2285,#2286,#1410,.T.);
#2679=EDGE_CURVE('',#2287,#2286,#1411,.T.);
#2680=EDGE_CURVE('',#2284,#2287,#1412,.T.);
#2681=EDGE_CURVE('',#2288,#2284,#1413,.T.);
#2682=EDGE_CURVE('',#2289,#2287,#1414,.T.);
#2683=EDGE_CURVE('',#2288,#2289,#1415,.T.);
#2684=EDGE_CURVE('',#2290,#2288,#1416,.T.);
#2685=EDGE_CURVE('',#2291,#2289,#1417,.T.);
#2686=EDGE_CURVE('',#2290,#2291,#1418,.T.);
#2687=EDGE_CURVE('',#2285,#2290,#1419,.T.);
#2688=EDGE_CURVE('',#2286,#2291,#1420,.T.);
#2689=EDGE_CURVE('',#2292,#2293,#1421,.T.);
#2690=EDGE_CURVE('',#2293,#2294,#1422,.T.);
#2691=EDGE_CURVE('',#2295,#2294,#1423,.T.);
#2692=EDGE_CURVE('',#2292,#2295,#1424,.T.);
#2693=EDGE_CURVE('',#2296,#2292,#1425,.T.);
#2694=EDGE_CURVE('',#2297,#2295,#1426,.T.);
#2695=EDGE_CURVE('',#2296,#2297,#1427,.T.);
#2696=EDGE_CURVE('',#2298,#2296,#1428,.T.);
#2697=EDGE_CURVE('',#2299,#2297,#1429,.T.);
#2698=EDGE_CURVE('',#2298,#2299,#1430,.T.);
#2699=EDGE_CURVE('',#2293,#2298,#1431,.T.);
#2700=EDGE_CURVE('',#2294,#2299,#1432,.T.);
#2701=EDGE_CURVE('',#2300,#2301,#1433,.T.);
#2702=EDGE_CURVE('',#2301,#2302,#1434,.T.);
#2703=EDGE_CURVE('',#2303,#2302,#1435,.T.);
#2704=EDGE_CURVE('',#2300,#2303,#1436,.T.);
#2705=EDGE_CURVE('',#2304,#2300,#1437,.T.);
#2706=EDGE_CURVE('',#2305,#2303,#1438,.T.);
#2707=EDGE_CURVE('',#2304,#2305,#1439,.T.);
#2708=EDGE_CURVE('',#2306,#2304,#1440,.T.);
#2709=EDGE_CURVE('',#2307,#2305,#1441,.T.);
#2710=EDGE_CURVE('',#2306,#2307,#1442,.T.);
#2711=EDGE_CURVE('',#2301,#2306,#1443,.T.);
#2712=EDGE_CURVE('',#2302,#2307,#1444,.T.);
#2713=EDGE_CURVE('',#2308,#2308,#2103,.T.);
#2714=EDGE_CURVE('',#2308,#2309,#1445,.T.);
#2715=EDGE_CURVE('',#2309,#2309,#2104,.T.);
#2716=EDGE_CURVE('',#2310,#2310,#2105,.T.);
#2717=EDGE_CURVE('',#2310,#2311,#1446,.T.);
#2718=EDGE_CURVE('',#2311,#2311,#2106,.T.);
#2719=EDGE_CURVE('',#2312,#2312,#2107,.T.);
#2720=EDGE_CURVE('',#2312,#2313,#1447,.T.);
#2721=EDGE_CURVE('',#2313,#2313,#2108,.T.);
#2722=EDGE_CURVE('',#2314,#2314,#2109,.T.);
#2723=EDGE_CURVE('',#2314,#2315,#1448,.T.);
#2724=EDGE_CURVE('',#2315,#2315,#2110,.T.);
#2725=EDGE_CURVE('',#2316,#2317,#1449,.T.);
#2726=EDGE_CURVE('',#2317,#2318,#1450,.T.);
#2727=EDGE_CURVE('',#2319,#2318,#1451,.T.);
#2728=EDGE_CURVE('',#2316,#2319,#1452,.T.);
#2729=EDGE_CURVE('',#2320,#2316,#1453,.T.);
#2730=EDGE_CURVE('',#2321,#2319,#1454,.T.);
#2731=EDGE_CURVE('',#2320,#2321,#1455,.T.);
#2732=EDGE_CURVE('',#2322,#2320,#1456,.T.);
#2733=EDGE_CURVE('',#2323,#2321,#1457,.T.);
#2734=EDGE_CURVE('',#2322,#2323,#1458,.T.);
#2735=EDGE_CURVE('',#2317,#2322,#1459,.T.);
#2736=EDGE_CURVE('',#2318,#2323,#1460,.T.);
#2737=EDGE_CURVE('',#2324,#2324,#2111,.T.);
#2738=EDGE_CURVE('',#2324,#2325,#1461,.T.);
#2739=EDGE_CURVE('',#2325,#2325,#2112,.T.);
#2740=EDGE_CURVE('',#2326,#2326,#2113,.T.);
#2741=EDGE_CURVE('',#2326,#2327,#1462,.T.);
#2742=EDGE_CURVE('',#2327,#2327,#2114,.T.);
#2743=EDGE_CURVE('',#2328,#2328,#2115,.T.);
#2744=EDGE_CURVE('',#2328,#2329,#1463,.T.);
#2745=EDGE_CURVE('',#2329,#2329,#2116,.T.);
#2746=EDGE_CURVE('',#2330,#2330,#2117,.T.);
#2747=EDGE_CURVE('',#2330,#2331,#1464,.T.);
#2748=EDGE_CURVE('',#2331,#2331,#2118,.T.);
#2749=EDGE_CURVE('',#2332,#2332,#2119,.T.);
#2750=EDGE_CURVE('',#2332,#2333,#1465,.T.);
#2751=EDGE_CURVE('',#2333,#2333,#2120,.T.);
#2752=EDGE_CURVE('',#2334,#2334,#2121,.T.);
#2753=EDGE_CURVE('',#2334,#2335,#1466,.T.);
#2754=EDGE_CURVE('',#2335,#2335,#2122,.T.);
#2755=EDGE_CURVE('',#2336,#2336,#2123,.T.);
#2756=EDGE_CURVE('',#2336,#2337,#1467,.T.);
#2757=EDGE_CURVE('',#2337,#2337,#2124,.T.);
#2758=EDGE_CURVE('',#2338,#2338,#2125,.T.);
#2759=EDGE_CURVE('',#2338,#2339,#1468,.T.);
#2760=EDGE_CURVE('',#2339,#2339,#2126,.T.);
#2761=EDGE_CURVE('',#2340,#2341,#1469,.T.);
#2762=EDGE_CURVE('',#2341,#2342,#1470,.T.);
#2763=EDGE_CURVE('',#2343,#2342,#1471,.T.);
#2764=EDGE_CURVE('',#2340,#2343,#1472,.T.);
#2765=EDGE_CURVE('',#2344,#2340,#1473,.T.);
#2766=EDGE_CURVE('',#2345,#2343,#1474,.T.);
#2767=EDGE_CURVE('',#2344,#2345,#1475,.T.);
#2768=EDGE_CURVE('',#2346,#2344,#1476,.T.);
#2769=EDGE_CURVE('',#2347,#2345,#1477,.T.);
#2770=EDGE_CURVE('',#2346,#2347,#1478,.T.);
#2771=EDGE_CURVE('',#2341,#2346,#1479,.T.);
#2772=EDGE_CURVE('',#2342,#2347,#1480,.T.);
#2773=EDGE_CURVE('',#2348,#2348,#2127,.T.);
#2774=EDGE_CURVE('',#2348,#2349,#1481,.T.);
#2775=EDGE_CURVE('',#2349,#2349,#2128,.T.);
#2776=EDGE_CURVE('',#2350,#2350,#2129,.T.);
#2777=EDGE_CURVE('',#2350,#2351,#1482,.T.);
#2778=EDGE_CURVE('',#2351,#2351,#2130,.T.);
#2779=EDGE_CURVE('',#2352,#2352,#2131,.T.);
#2780=EDGE_CURVE('',#2352,#2353,#1483,.T.);
#2781=EDGE_CURVE('',#2353,#2353,#2132,.T.);
#2782=EDGE_CURVE('',#2354,#2354,#2133,.T.);
#2783=EDGE_CURVE('',#2354,#2355,#1484,.T.);
#2784=EDGE_CURVE('',#2355,#2355,#2134,.T.);
#2785=EDGE_CURVE('',#2356,#2356,#2135,.T.);
#2786=EDGE_CURVE('',#2356,#2357,#1485,.T.);
#2787=EDGE_CURVE('',#2357,#2357,#2136,.T.);
#2788=EDGE_CURVE('',#2358,#2358,#2137,.T.);
#2789=EDGE_CURVE('',#2358,#2359,#1486,.T.);
#2790=EDGE_CURVE('',#2359,#2359,#2138,.T.);
#2791=EDGE_CURVE('',#2360,#2361,#2139,.T.);
#2792=EDGE_CURVE('',#2362,#2363,#1487,.T.);
#2793=EDGE_CURVE('',#2362,#2364,#1488,.T.);
#2794=EDGE_CURVE('',#2363,#2364,#2140,.T.);
#2795=EDGE_CURVE('',#2365,#2366,#1489,.T.);
#2796=EDGE_CURVE('',#2367,#2365,#2141,.T.);
#2797=EDGE_CURVE('',#2367,#2366,#1490,.T.);
#2798=EDGE_CURVE('',#2368,#2369,#1491,.T.);
#2799=EDGE_CURVE('',#2370,#2368,#2142,.T.);
#2800=EDGE_CURVE('',#2370,#2369,#1492,.T.);
#2801=EDGE_CURVE('',#2369,#2362,#1493,.T.);
#2802=EDGE_CURVE('',#2364,#2370,#1494,.T.);
#2803=EDGE_CURVE('',#2371,#2372,#1495,.T.);
#2804=EDGE_CURVE('',#2371,#2373,#1496,.T.);
#2805=EDGE_CURVE('',#2372,#2373,#2143,.T.);
#2806=EDGE_CURVE('',#2366,#2371,#1497,.T.);
#2807=EDGE_CURVE('',#2373,#2367,#1498,.T.);
#2808=EDGE_CURVE('',#2374,#2375,#1499,.T.);
#2809=EDGE_CURVE('',#2375,#2376,#1500,.T.);
#2810=EDGE_CURVE('',#2376,#2377,#1501,.T.);
#2811=EDGE_CURVE('',#2377,#2374,#1502,.T.);
#2812=EDGE_CURVE('',#2378,#2378,#2144,.T.);
#2813=EDGE_CURVE('',#2379,#2379,#2145,.T.);
#2814=EDGE_CURVE('',#2372,#2380,#1503,.T.);
#2815=EDGE_CURVE('',#2380,#2381,#1504,.T.);
#2816=EDGE_CURVE('',#2381,#2368,#1505,.T.);
#2817=EDGE_CURVE('',#2363,#2382,#1506,.T.);
#2818=EDGE_CURVE('',#2382,#2383,#1507,.T.);
#2819=EDGE_CURVE('',#2383,#2365,#1508,.T.);
#2820=EDGE_CURVE('',#2382,#2383,#2146,.T.);
#2821=EDGE_CURVE('',#2380,#2381,#2147,.T.);
#2822=EDGE_CURVE('',#2384,#2385,#1509,.T.);
#2823=EDGE_CURVE('',#2384,#2386,#1510,.T.);
#2824=EDGE_CURVE('',#2386,#2387,#1511,.T.);
#2825=EDGE_CURVE('',#2385,#2387,#1512,.T.);
#2826=EDGE_CURVE('',#2388,#2384,#1513,.T.);
#2827=EDGE_CURVE('',#2388,#2389,#1514,.T.);
#2828=EDGE_CURVE('',#2389,#2386,#1515,.T.);
#2829=EDGE_CURVE('',#2390,#2388,#1516,.T.);
#2830=EDGE_CURVE('',#2390,#2391,#1517,.T.);
#2831=EDGE_CURVE('',#2391,#2389,#1518,.T.);
#2832=EDGE_CURVE('',#2385,#2390,#1519,.T.);
#2833=EDGE_CURVE('',#2387,#2391,#1520,.T.);
#2834=EDGE_CURVE('',#2392,#2392,#2148,.T.);
#2835=EDGE_CURVE('',#2392,#2379,#1521,.T.);
#2836=EDGE_CURVE('',#2393,#2393,#2149,.T.);
#2837=EDGE_CURVE('',#2393,#2378,#1522,.T.);
#2838=EDGE_CURVE('',#2394,#2395,#1523,.T.);
#2839=EDGE_CURVE('',#2395,#2374,#1524,.T.);
#2840=EDGE_CURVE('',#2394,#2377,#1525,.T.);
#2841=EDGE_CURVE('',#2396,#2394,#1526,.T.);
#2842=EDGE_CURVE('',#2396,#2376,#1527,.T.);
#2843=EDGE_CURVE('',#2397,#2396,#1528,.T.);
#2844=EDGE_CURVE('',#2397,#2375,#1529,.T.);
#2845=EDGE_CURVE('',#2395,#2397,#1530,.T.);
#2846=EDGE_CURVE('',#2398,#2398,#2150,.T.);
#2847=EDGE_CURVE('',#2398,#2399,#1531,.T.);
#2848=EDGE_CURVE('',#2399,#2399,#2151,.T.);
#2849=EDGE_CURVE('',#2400,#2400,#2152,.T.);
#2850=EDGE_CURVE('',#2401,#2402,#2153,.T.);
#2851=EDGE_CURVE('',#2403,#2403,#2154,.T.);
#2852=EDGE_CURVE('',#2404,#2405,#300,.T.);
#2853=EDGE_CURVE('',#2406,#2404,#301,.T.);
#2854=EDGE_CURVE('',#2405,#2406,#302,.T.);
#2855=EDGE_CURVE('',#2405,#2407,#1532,.T.);
#2856=EDGE_CURVE('',#2407,#2407,#303,.T.);
#2857=EDGE_CURVE('',#2408,#2408,#304,.T.);
#2858=EDGE_CURVE('',#2408,#2409,#1533,.T.);
#2859=EDGE_CURVE('',#2410,#2409,#305,.T.);
#2860=EDGE_CURVE('',#2411,#2410,#306,.T.);
#2861=EDGE_CURVE('',#2409,#2411,#307,.T.);
#2862=EDGE_CURVE('',#2412,#2412,#2155,.T.);
#2863=EDGE_CURVE('',#2412,#2413,#1534,.T.);
#2864=EDGE_CURVE('',#2413,#2413,#2156,.T.);
#2865=EDGE_CURVE('',#2414,#2415,#308,.T.);
#2866=EDGE_CURVE('',#2415,#2416,#309,.T.);
#2867=EDGE_CURVE('',#2416,#2414,#310,.T.);
#2868=EDGE_CURVE('',#2417,#2418,#311,.T.);
#2869=EDGE_CURVE('',#2418,#2419,#312,.T.);
#2870=EDGE_CURVE('',#2419,#2417,#313,.T.);
#2871=EDGE_CURVE('',#2420,#2421,#314,.T.);
#2872=EDGE_CURVE('',#2421,#2422,#315,.T.);
#2873=EDGE_CURVE('',#2422,#2420,#316,.T.);
#2874=EDGE_CURVE('',#2423,#2424,#317,.T.);
#2875=EDGE_CURVE('',#2424,#2425,#318,.T.);
#2876=EDGE_CURVE('',#2425,#2423,#319,.T.);
#2877=EDGE_CURVE('',#2416,#2426,#1535,.T.);
#2878=EDGE_CURVE('',#2426,#2426,#320,.T.);
#2879=EDGE_CURVE('',#2427,#2427,#321,.T.);
#2880=EDGE_CURVE('',#2427,#2419,#1536,.T.);
#2881=EDGE_CURVE('',#2422,#2428,#1537,.T.);
#2882=EDGE_CURVE('',#2428,#2428,#322,.T.);
#2883=EDGE_CURVE('',#2429,#2429,#323,.T.);
#2884=EDGE_CURVE('',#2429,#2425,#1538,.T.);
#2885=EDGE_CURVE('',#2430,#2430,#2157,.T.);
#2886=EDGE_CURVE('',#2431,#2431,#2158,.T.);
#2887=EDGE_CURVE('',#2432,#2432,#2159,.T.);
#2888=EDGE_CURVE('',#2432,#2431,#1539,.T.);
#2889=EDGE_CURVE('',#2433,#2433,#2160,.T.);
#2890=EDGE_CURVE('',#2433,#2430,#1540,.T.);
#2891=EDGE_CURVE('',#2434,#2434,#2161,.T.);
#2892=EDGE_CURVE('',#2434,#2435,#1541,.T.);
#2893=EDGE_CURVE('',#2435,#2435,#2162,.T.);
#2894=EDGE_CURVE('',#2436,#2436,#2163,.T.);
#2895=EDGE_CURVE('',#2436,#2437,#1542,.T.);
#2896=EDGE_CURVE('',#2437,#2437,#2164,.T.);
#2897=EDGE_CURVE('',#2438,#2439,#1543,.T.);
#2898=EDGE_CURVE('',#2439,#2440,#1544,.T.);
#2899=EDGE_CURVE('',#2440,#2441,#1545,.T.);
#2900=EDGE_CURVE('',#2438,#2441,#1546,.T.);
#2901=EDGE_CURVE('',#2439,#2442,#1547,.T.);
#2902=EDGE_CURVE('',#2442,#2443,#1548,.T.);
#2903=EDGE_CURVE('',#2443,#2440,#1549,.T.);
#2904=EDGE_CURVE('',#2442,#2444,#1550,.T.);
#2905=EDGE_CURVE('',#2444,#2445,#1551,.T.);
#2906=EDGE_CURVE('',#2445,#2443,#1552,.T.);
#2907=EDGE_CURVE('',#2444,#2446,#1553,.T.);
#2908=EDGE_CURVE('',#2446,#2447,#1554,.T.);
#2909=EDGE_CURVE('',#2447,#2445,#1555,.T.);
#2910=EDGE_CURVE('',#2446,#2448,#1556,.T.);
#2911=EDGE_CURVE('',#2448,#2449,#1557,.T.);
#2912=EDGE_CURVE('',#2449,#2447,#1558,.T.);
#2913=EDGE_CURVE('',#2448,#2438,#1559,.T.);
#2914=EDGE_CURVE('',#2441,#2449,#1560,.T.);
#2915=EDGE_CURVE('',#2450,#2450,#2165,.T.);
#2916=EDGE_CURVE('',#2451,#2451,#2166,.T.);
#2917=EDGE_CURVE('',#2452,#2452,#2167,.T.);
#2918=EDGE_CURVE('',#2452,#2451,#1561,.T.);
#2919=EDGE_CURVE('',#2453,#2453,#2168,.T.);
#2920=EDGE_CURVE('',#2453,#2452,#1562,.T.);
#2921=EDGE_CURVE('',#2454,#2454,#2169,.T.);
#2922=EDGE_CURVE('',#2454,#2453,#1563,.T.);
#2923=EDGE_CURVE('',#2455,#2455,#2170,.T.);
#2924=EDGE_CURVE('',#2456,#2456,#2171,.F.);
#2925=EDGE_CURVE('',#2456,#2455,#1564,.T.);
#2926=EDGE_CURVE('',#2450,#2456,#1565,.T.);
#2927=EDGE_CURVE('',#2457,#2457,#2172,.T.);
#2928=EDGE_CURVE('',#2457,#2458,#1566,.T.);
#2929=EDGE_CURVE('',#2458,#2458,#2173,.T.);
#2930=EDGE_CURVE('',#2459,#2460,#1567,.T.);
#2931=EDGE_CURVE('',#2459,#2461,#1568,.T.);
#2932=EDGE_CURVE('',#2462,#2461,#1569,.T.);
#2933=EDGE_CURVE('',#2462,#2460,#1570,.T.);
#2934=EDGE_CURVE('',#2460,#2463,#2174,.T.);
#2935=EDGE_CURVE('',#2464,#2462,#1571,.T.);
#2936=EDGE_CURVE('',#2463,#2464,#1572,.T.);
#2937=EDGE_CURVE('',#2463,#2465,#1573,.T.);
#2938=EDGE_CURVE('',#2464,#2466,#1574,.T.);
#2939=EDGE_CURVE('',#2466,#2465,#1575,.T.);
#2940=EDGE_CURVE('',#2461,#2466,#1576,.T.);
#2941=EDGE_CURVE('',#2465,#2459,#2175,.T.);
#2942=EDGE_CURVE('',#2467,#2467,#2176,.T.);
#2943=EDGE_CURVE('',#2467,#2468,#1577,.T.);
#2944=EDGE_CURVE('',#2468,#2468,#2177,.T.);
#2945=EDGE_CURVE('',#2469,#2469,#2178,.T.);
#2946=EDGE_CURVE('',#2469,#2470,#1578,.T.);
#2947=EDGE_CURVE('',#2470,#2470,#2179,.T.);
#2948=EDGE_CURVE('',#2471,#2471,#2180,.T.);
#2949=EDGE_CURVE('',#2471,#2472,#1579,.T.);
#2950=EDGE_CURVE('',#2472,#2472,#2181,.T.);
#2951=EDGE_CURVE('',#2473,#2473,#2182,.T.);
#2952=EDGE_CURVE('',#2473,#2474,#1580,.T.);
#2953=EDGE_CURVE('',#2474,#2474,#2183,.T.);
#2954=EDGE_CURVE('',#2475,#2475,#2184,.T.);
#2955=EDGE_CURVE('',#2475,#2476,#1581,.T.);
#2956=EDGE_CURVE('',#2476,#2476,#2185,.T.);
#2957=EDGE_CURVE('',#2477,#2478,#1582,.T.);
#2958=EDGE_CURVE('',#2477,#2478,#2186,.T.);
#2959=EDGE_CURVE('',#2479,#2477,#324,.T.);
#2960=EDGE_CURVE('',#2480,#2479,#2187,.T.);
#2961=EDGE_CURVE('',#2480,#2481,#1583,.T.);
#2962=EDGE_CURVE('',#2482,#2481,#325,.T.);
#2963=EDGE_CURVE('',#2481,#2482,#326,.T.);
#2964=EDGE_CURVE('',#2483,#2480,#2188,.T.);
#2965=EDGE_CURVE('',#2478,#2483,#327,.T.);
#2966=EDGE_CURVE('',#2483,#2479,#1584,.T.);
#2967=EDGE_CURVE('',#2484,#2485,#1585,.T.);
#2968=EDGE_CURVE('',#2484,#2486,#1586,.T.);
#2969=EDGE_CURVE('',#2487,#2486,#1587,.T.);
#2970=EDGE_CURVE('',#2485,#2487,#1588,.T.);
#2971=EDGE_CURVE('',#2488,#2484,#1589,.T.);
#2972=EDGE_CURVE('',#2488,#2489,#1590,.T.);
#2973=EDGE_CURVE('',#2486,#2489,#1591,.T.);
#2974=EDGE_CURVE('',#2490,#2488,#1592,.T.);
#2975=EDGE_CURVE('',#2491,#2490,#1593,.T.);
#2976=EDGE_CURVE('',#2489,#2491,#1594,.T.);
#2977=EDGE_CURVE('',#2492,#2492,#2189,.T.);
#2978=EDGE_CURVE('',#2490,#2485,#2190,.T.);
#2979=EDGE_CURVE('',#2493,#2493,#2191,.T.);
#2980=EDGE_CURVE('',#2493,#2494,#1595,.T.);
#2981=EDGE_CURVE('',#2494,#2494,#2192,.T.);
#2982=EDGE_CURVE('',#2487,#2491,#2193,.T.);
#2983=EDGE_CURVE('',#2495,#2495,#2194,.T.);
#2984=EDGE_CURVE('',#2496,#2496,#2195,.T.);
#2985=EDGE_CURVE('',#2497,#2497,#2196,.T.);
#2986=EDGE_CURVE('',#2497,#2495,#1596,.T.);
#2987=EDGE_CURVE('',#2496,#2492,#1597,.T.);
#2988=EDGE_CURVE('',#2498,#2498,#2197,.T.);
#2989=EDGE_CURVE('',#2498,#2499,#1598,.T.);
#2990=EDGE_CURVE('',#2499,#2499,#2198,.T.);
#2991=EDGE_CURVE('',#2500,#2500,#2199,.T.);
#2992=EDGE_CURVE('',#2500,#2501,#1599,.T.);
#2993=EDGE_CURVE('',#2501,#2501,#2200,.T.);
#2994=EDGE_CURVE('',#2502,#2502,#2201,.T.);
#2995=EDGE_CURVE('',#2502,#2503,#1600,.T.);
#2996=EDGE_CURVE('',#2503,#2503,#2202,.T.);
#2997=EDGE_CURVE('',#2504,#2505,#1601,.T.);
#2998=EDGE_CURVE('',#2504,#2506,#1602,.T.);
#2999=EDGE_CURVE('',#2507,#2506,#1603,.T.);
#3000=EDGE_CURVE('',#2507,#2505,#1604,.T.);
#3001=EDGE_CURVE('',#2505,#2508,#2203,.T.);
#3002=EDGE_CURVE('',#2509,#2507,#1605,.T.);
#3003=EDGE_CURVE('',#2508,#2509,#1606,.T.);
#3004=EDGE_CURVE('',#2508,#2510,#1607,.T.);
#3005=EDGE_CURVE('',#2509,#2511,#1608,.T.);
#3006=EDGE_CURVE('',#2511,#2510,#1609,.T.);
#3007=EDGE_CURVE('',#2506,#2511,#1610,.T.);
#3008=EDGE_CURVE('',#2510,#2504,#2204,.T.);
#3009=EDGE_CURVE('',#2512,#2512,#2205,.T.);
#3010=EDGE_CURVE('',#2512,#2513,#1611,.T.);
#3011=EDGE_CURVE('',#2513,#2513,#2206,.T.);
#3012=EDGE_CURVE('',#2514,#2514,#2207,.T.);
#3013=EDGE_CURVE('',#2514,#2515,#1612,.T.);
#3014=EDGE_CURVE('',#2515,#2515,#2208,.T.);
#3015=EDGE_CURVE('',#2516,#2516,#2209,.T.);
#3016=EDGE_CURVE('',#2516,#2517,#1613,.T.);
#3017=EDGE_CURVE('',#2517,#2517,#2210,.T.);
#3018=EDGE_CURVE('',#2518,#2518,#2211,.T.);
#3019=EDGE_CURVE('',#2518,#2519,#1614,.T.);
#3020=EDGE_CURVE('',#2519,#2519,#2212,.T.);
#3021=EDGE_CURVE('',#2520,#2520,#2213,.T.);
#3022=EDGE_CURVE('',#2520,#2521,#1615,.T.);
#3023=EDGE_CURVE('',#2521,#2521,#2214,.T.);
#3024=EDGE_CURVE('',#2522,#2523,#1616,.T.);
#3025=EDGE_CURVE('',#2522,#2523,#2215,.T.);
#3026=EDGE_CURVE('',#2524,#2522,#328,.T.);
#3027=EDGE_CURVE('',#2525,#2524,#2216,.T.);
#3028=EDGE_CURVE('',#2525,#2526,#1617,.T.);
#3029=EDGE_CURVE('',#2527,#2526,#329,.T.);
#3030=EDGE_CURVE('',#2526,#2527,#330,.T.);
#3031=EDGE_CURVE('',#2528,#2525,#2217,.T.);
#3032=EDGE_CURVE('',#2523,#2528,#331,.T.);
#3033=EDGE_CURVE('',#2528,#2524,#1618,.T.);
#3034=EDGE_CURVE('',#2529,#2530,#1619,.T.);
#3035=EDGE_CURVE('',#2531,#2529,#1620,.T.);
#3036=EDGE_CURVE('',#2532,#2531,#1621,.T.);
#3037=EDGE_CURVE('',#2530,#2532,#1622,.T.);
#3038=EDGE_CURVE('',#2533,#2534,#1623,.T.);
#3039=EDGE_CURVE('',#2535,#2533,#1624,.T.);
#3040=EDGE_CURVE('',#2536,#2535,#1625,.T.);
#3041=EDGE_CURVE('',#2536,#2534,#1626,.T.);
#3042=EDGE_CURVE('',#2534,#2529,#1627,.T.);
#3043=EDGE_CURVE('',#2531,#2536,#1628,.T.);
#3044=EDGE_CURVE('',#2537,#2537,#2218,.T.);
#3045=EDGE_CURVE('',#2532,#2535,#2219,.T.);
#3046=EDGE_CURVE('',#2530,#2533,#2220,.T.);
#3047=EDGE_CURVE('',#2538,#2538,#2221,.T.);
#3048=EDGE_CURVE('',#2538,#2537,#1629,.T.);
#3049=EDGE_CURVE('',#2539,#2539,#2222,.T.);
#3050=EDGE_CURVE('',#2540,#2540,#2223,.T.);
#3051=EDGE_CURVE('',#2539,#2541,#1630,.T.);
#3052=EDGE_CURVE('',#2541,#2541,#2224,.T.);
#3053=EDGE_CURVE('',#2542,#2542,#2225,.T.);
#3054=EDGE_CURVE('',#2542,#2540,#1631,.T.);
#3055=EDGE_CURVE('',#2543,#2543,#2226,.T.);
#3056=EDGE_CURVE('',#2543,#2544,#1632,.T.);
#3057=EDGE_CURVE('',#2544,#2544,#2227,.T.);
#3058=EDGE_CURVE('',#2545,#2545,#2228,.T.);
#3059=EDGE_CURVE('',#2545,#2546,#1633,.T.);
#3060=EDGE_CURVE('',#2546,#2546,#2229,.T.);
#3061=EDGE_CURVE('',#2547,#2547,#2230,.T.);
#3062=EDGE_CURVE('',#2547,#2548,#1634,.T.);
#3063=EDGE_CURVE('',#2548,#2548,#2231,.T.);
#3064=EDGE_CURVE('',#2549,#2549,#2232,.T.);
#3065=EDGE_CURVE('',#2549,#2550,#1635,.T.);
#3066=EDGE_CURVE('',#2550,#2550,#2233,.T.);
#3067=EDGE_CURVE('',#2551,#2552,#1636,.T.);
#3068=EDGE_CURVE('',#2551,#2552,#2234,.T.);
#3069=EDGE_CURVE('',#2553,#2551,#332,.T.);
#3070=EDGE_CURVE('',#2554,#2553,#2235,.T.);
#3071=EDGE_CURVE('',#2554,#2555,#1637,.T.);
#3072=EDGE_CURVE('',#2556,#2555,#333,.T.);
#3073=EDGE_CURVE('',#2555,#2556,#334,.T.);
#3074=EDGE_CURVE('',#2557,#2554,#2236,.T.);
#3075=EDGE_CURVE('',#2552,#2557,#335,.T.);
#3076=EDGE_CURVE('',#2557,#2553,#1638,.T.);
#3077=EDGE_CURVE('',#2558,#2558,#2237,.T.);
#3078=EDGE_CURVE('',#2558,#2559,#1639,.T.);
#3079=EDGE_CURVE('',#2559,#2559,#2238,.T.);
#3080=EDGE_CURVE('',#2560,#2560,#2239,.T.);
#3081=EDGE_CURVE('',#2560,#2561,#1640,.T.);
#3082=EDGE_CURVE('',#2561,#2561,#2240,.T.);
#3083=EDGE_CURVE('',#2562,#2563,#1641,.T.);
#3084=EDGE_CURVE('',#2562,#2563,#2241,.T.);
#3085=EDGE_CURVE('',#2564,#2562,#336,.T.);
#3086=EDGE_CURVE('',#2565,#2564,#2242,.T.);
#3087=EDGE_CURVE('',#2565,#2566,#1642,.T.);
#3088=EDGE_CURVE('',#2567,#2566,#337,.T.);
#3089=EDGE_CURVE('',#2566,#2567,#338,.T.);
#3090=EDGE_CURVE('',#2568,#2565,#2243,.T.);
#3091=EDGE_CURVE('',#2563,#2568,#339,.T.);
#3092=EDGE_CURVE('',#2568,#2564,#1643,.T.);
#3093=EDGE_CURVE('',#2569,#2569,#2244,.T.);
#3094=EDGE_CURVE('',#2569,#2570,#1644,.T.);
#3095=EDGE_CURVE('',#2570,#2570,#2245,.T.);
#3096=EDGE_CURVE('',#2571,#2571,#2246,.T.);
#3097=EDGE_CURVE('',#2571,#2572,#1645,.T.);
#3098=EDGE_CURVE('',#2572,#2572,#2247,.T.);
#3099=EDGE_CURVE('',#2573,#2574,#1646,.T.);
#3100=EDGE_CURVE('',#2575,#2573,#1647,.T.);
#3101=EDGE_CURVE('',#2576,#2575,#1648,.T.);
#3102=EDGE_CURVE('',#2577,#2576,#1649,.T.);
#3103=EDGE_CURVE('',#2578,#2577,#1650,.T.);
#3104=EDGE_CURVE('',#2579,#2578,#1651,.T.);
#3105=EDGE_CURVE('',#2580,#2579,#1652,.T.);
#3106=EDGE_CURVE('',#2574,#2580,#1653,.T.);
#3107=EDGE_CURVE('',#2577,#2581,#1654,.T.);
#3108=EDGE_CURVE('',#2581,#2582,#1655,.T.);
#3109=EDGE_CURVE('',#2582,#2578,#1656,.T.);
#3110=EDGE_CURVE('',#2583,#2576,#1657,.T.);
#3111=EDGE_CURVE('',#2583,#2581,#1658,.T.);
#3112=EDGE_CURVE('',#2575,#2584,#1659,.T.);
#3113=EDGE_CURVE('',#2584,#2583,#1660,.T.);
#3114=EDGE_CURVE('',#2585,#2573,#1661,.T.);
#3115=EDGE_CURVE('',#2585,#2584,#1662,.T.);
#3116=EDGE_CURVE('',#2586,#2587,#1663,.T.);
#3117=EDGE_CURVE('',#2582,#2586,#1664,.T.);
#3118=EDGE_CURVE('',#2588,#2585,#1665,.T.);
#3119=EDGE_CURVE('',#2587,#2588,#1666,.T.);
#3120=EDGE_CURVE('',#2579,#2586,#1667,.T.);
#3121=EDGE_CURVE('',#2574,#2588,#1668,.T.);
#3122=EDGE_CURVE('',#2587,#2580,#1669,.T.);
#3123=EDGE_CURVE('',#2589,#2589,#2248,.T.);
#3124=EDGE_CURVE('',#2590,#2590,#2249,.T.);
#3125=EDGE_CURVE('',#2590,#2589,#1670,.T.);
#3126=EDGE_CURVE('',#2591,#2591,#2250,.T.);
#3127=EDGE_CURVE('',#2591,#2590,#1671,.T.);
#3128=EDGE_CURVE('',#2592,#2592,#2251,.T.);
#3129=EDGE_CURVE('',#2592,#2591,#1672,.T.);
#3130=EDGE_CURVE('',#2593,#2593,#2252,.T.);
#3131=EDGE_CURVE('',#2594,#2594,#2253,.F.);
#3132=EDGE_CURVE('',#2594,#2593,#1673,.T.);
#3133=EDGE_CURVE('',#2595,#2595,#2254,.F.);
#3134=EDGE_CURVE('',#2595,#2594,#1674,.T.);
#3135=EDGE_CURVE('',#2596,#2596,#2255,.T.);
#3136=EDGE_CURVE('',#2596,#2595,#1675,.T.);
#3137=EDGE_CURVE('',#2597,#2598,#1676,.T.);
#3138=EDGE_CURVE('',#2598,#2599,#1677,.T.);
#3139=EDGE_CURVE('',#2599,#2600,#1678,.T.);
#3140=EDGE_CURVE('',#2597,#2600,#1679,.T.);
#3141=EDGE_CURVE('',#2598,#2601,#1680,.T.);
#3142=EDGE_CURVE('',#2601,#2602,#1681,.T.);
#3143=EDGE_CURVE('',#2602,#2599,#1682,.T.);
#3144=EDGE_CURVE('',#2601,#2603,#1683,.T.);
#3145=EDGE_CURVE('',#2603,#2604,#1684,.T.);
#3146=EDGE_CURVE('',#2604,#2602,#1685,.T.);
#3147=EDGE_CURVE('',#2603,#2605,#1686,.T.);
#3148=EDGE_CURVE('',#2605,#2606,#1687,.T.);
#3149=EDGE_CURVE('',#2606,#2604,#1688,.T.);
#3150=EDGE_CURVE('',#2605,#2607,#1689,.T.);
#3151=EDGE_CURVE('',#2607,#2608,#1690,.T.);
#3152=EDGE_CURVE('',#2608,#2606,#1691,.T.);
#3153=EDGE_CURVE('',#2607,#2597,#1692,.T.);
#3154=EDGE_CURVE('',#2600,#2608,#1693,.T.);
#3155=EDGE_CURVE('',#2609,#2609,#2256,.T.);
#3156=EDGE_CURVE('',#2610,#2610,#2257,.T.);
#3157=EDGE_CURVE('',#2610,#2609,#1694,.T.);
#3158=EDGE_CURVE('',#2611,#2611,#2258,.T.);
#3159=EDGE_CURVE('',#2611,#2610,#1695,.T.);
#3160=EDGE_CURVE('',#2612,#2612,#2259,.T.);
#3161=EDGE_CURVE('',#2612,#2611,#1696,.T.);
#3162=EDGE_CURVE('',#2613,#2613,#2260,.T.);
#3163=EDGE_CURVE('',#2614,#2614,#2261,.F.);
#3164=EDGE_CURVE('',#2614,#2613,#1697,.T.);
#3165=EDGE_CURVE('',#2615,#2615,#2262,.F.);
#3166=EDGE_CURVE('',#2615,#2614,#1698,.T.);
#3167=EDGE_CURVE('',#2616,#2616,#2263,.T.);
#3168=EDGE_CURVE('',#2616,#2615,#1699,.T.);
#3169=EDGE_CURVE('',#2617,#2618,#1700,.T.);
#3170=EDGE_CURVE('',#2618,#2619,#1701,.T.);
#3171=EDGE_CURVE('',#2619,#2620,#1702,.T.);
#3172=EDGE_CURVE('',#2617,#2620,#1703,.T.);
#3173=EDGE_CURVE('',#2618,#2621,#1704,.T.);
#3174=EDGE_CURVE('',#2621,#2622,#1705,.T.);
#3175=EDGE_CURVE('',#2622,#2619,#1706,.T.);
#3176=EDGE_CURVE('',#2621,#2623,#1707,.T.);
#3177=EDGE_CURVE('',#2623,#2624,#1708,.T.);
#3178=EDGE_CURVE('',#2624,#2622,#1709,.T.);
#3179=EDGE_CURVE('',#2623,#2625,#1710,.T.);
#3180=EDGE_CURVE('',#2625,#2626,#1711,.T.);
#3181=EDGE_CURVE('',#2626,#2624,#1712,.T.);
#3182=EDGE_CURVE('',#2625,#2627,#1713,.T.);
#3183=EDGE_CURVE('',#2627,#2628,#1714,.T.);
#3184=EDGE_CURVE('',#2628,#2626,#1715,.T.);
#3185=EDGE_CURVE('',#2627,#2617,#1716,.T.);
#3186=EDGE_CURVE('',#2620,#2628,#1717,.T.);
#3187=EDGE_CURVE('',#2629,#2629,#2264,.T.);
#3188=EDGE_CURVE('',#2629,#2630,#1718,.T.);
#3189=EDGE_CURVE('',#2630,#2630,#2265,.T.);
#3190=EDGE_CURVE('',#2631,#2631,#2266,.T.);
#3191=EDGE_CURVE('',#2631,#2632,#1719,.T.);
#3192=EDGE_CURVE('',#2632,#2632,#2267,.T.);
#3193=EDGE_CURVE('',#2633,#2634,#11,.T.);
#3194=EDGE_CURVE('',#2635,#2633,#12,.T.);
#3195=EDGE_CURVE('',#2635,#2636,#1720,.T.);
#3196=EDGE_CURVE('',#2636,#2636,#2268,.T.);
#3197=EDGE_CURVE('',#2637,#2635,#13,.T.);
#3198=EDGE_CURVE('',#2638,#2637,#14,.T.);
#3199=EDGE_CURVE('',#2639,#2638,#15,.T.);
#3200=EDGE_CURVE('',#2634,#2639,#16,.T.);
#3201=EDGE_CURVE('',#2640,#2640,#2269,.T.);
#3202=EDGE_CURVE('',#2640,#2641,#1721,.T.);
#3203=EDGE_CURVE('',#2642,#2641,#17,.T.);
#3204=EDGE_CURVE('',#2643,#2642,#18,.T.);
#3205=EDGE_CURVE('',#2644,#2643,#19,.T.);
#3206=EDGE_CURVE('',#2645,#2644,#20,.T.);
#3207=EDGE_CURVE('',#2646,#2645,#21,.T.);
#3208=EDGE_CURVE('',#2641,#2646,#22,.T.);
#3209=EDGE_CURVE('',#2637,#2646,#1722,.T.);
#3210=EDGE_CURVE('',#2638,#2645,#1723,.T.);
#3211=EDGE_CURVE('',#2635,#2641,#1724,.T.);
#3212=EDGE_CURVE('',#2633,#2642,#1725,.T.);
#3213=EDGE_CURVE('',#2647,#2647,#2270,.F.);
#3214=EDGE_CURVE('',#2647,#2648,#1726,.T.);
#3215=EDGE_CURVE('',#2648,#2648,#2271,.F.);
#3216=EDGE_CURVE('',#2634,#2643,#1727,.T.);
#3217=EDGE_CURVE('',#2639,#2644,#1728,.T.);
#3218=EDGE_CURVE('',#2649,#2650,#1729,.T.);
#3219=EDGE_CURVE('',#2649,#2651,#1730,.T.);
#3220=EDGE_CURVE('',#2651,#2652,#1731,.T.);
#3221=EDGE_CURVE('',#2650,#2652,#1732,.T.);
#3222=EDGE_CURVE('',#2653,#2649,#1733,.T.);
#3223=EDGE_CURVE('',#2653,#2654,#1734,.T.);
#3224=EDGE_CURVE('',#2654,#2651,#1735,.T.);
#3225=EDGE_CURVE('',#2655,#2653,#1736,.T.);
#3226=EDGE_CURVE('',#2655,#2656,#1737,.T.);
#3227=EDGE_CURVE('',#2656,#2654,#1738,.T.);
#3228=EDGE_CURVE('',#2657,#2655,#1739,.T.);
#3229=EDGE_CURVE('',#2657,#2658,#1740,.T.);
#3230=EDGE_CURVE('',#2658,#2656,#1741,.T.);
#3231=EDGE_CURVE('',#2659,#2657,#1742,.T.);
#3232=EDGE_CURVE('',#2659,#2660,#1743,.T.);
#3233=EDGE_CURVE('',#2660,#2658,#1744,.T.);
#3234=EDGE_CURVE('',#2650,#2659,#1745,.T.);
#3235=EDGE_CURVE('',#2652,#2660,#1746,.T.);
#3236=EDGE_CURVE('',#2661,#2661,#2272,.T.);
#3237=EDGE_CURVE('',#2662,#2662,#2273,.T.);
#3238=EDGE_CURVE('',#2662,#2661,#1747,.T.);
#3239=EDGE_CURVE('',#2663,#2663,#2274,.F.);
#3240=EDGE_CURVE('',#2663,#2662,#1748,.T.);
#3241=EDGE_CURVE('',#2664,#2664,#2275,.T.);
#3242=EDGE_CURVE('',#2664,#2663,#1749,.T.);
#3243=ORIENTED_EDGE('',*,*,#2665,.F.);
#3244=ORIENTED_EDGE('',*,*,#2666,.T.);
#3245=ORIENTED_EDGE('',*,*,#2667,.F.);
#3246=ORIENTED_EDGE('',*,*,#2666,.F.);
#3247=ORIENTED_EDGE('',*,*,#2668,.F.);
#3248=ORIENTED_EDGE('',*,*,#2669,.T.);
#3249=ORIENTED_EDGE('',*,*,#2670,.F.);
#3250=ORIENTED_EDGE('',*,*,#2669,.F.);
#3251=ORIENTED_EDGE('',*,*,#2671,.F.);
#3252=ORIENTED_EDGE('',*,*,#2672,.T.);
#3253=ORIENTED_EDGE('',*,*,#2673,.F.);
#3254=ORIENTED_EDGE('',*,*,#2672,.F.);
#3255=ORIENTED_EDGE('',*,*,#2674,.F.);
#3256=ORIENTED_EDGE('',*,*,#2675,.T.);
#3257=ORIENTED_EDGE('',*,*,#2676,.F.);
#3258=ORIENTED_EDGE('',*,*,#2675,.F.);
#3259=ORIENTED_EDGE('',*,*,#2677,.T.);
#3260=ORIENTED_EDGE('',*,*,#2678,.T.);
#3261=ORIENTED_EDGE('',*,*,#2679,.F.);
#3262=ORIENTED_EDGE('',*,*,#2680,.F.);
#3263=ORIENTED_EDGE('',*,*,#2681,.T.);
#3264=ORIENTED_EDGE('',*,*,#2680,.T.);
#3265=ORIENTED_EDGE('',*,*,#2682,.F.);
#3266=ORIENTED_EDGE('',*,*,#2683,.F.);
#3267=ORIENTED_EDGE('',*,*,#2684,.T.);
#3268=ORIENTED_EDGE('',*,*,#2683,.T.);
#3269=ORIENTED_EDGE('',*,*,#2685,.F.);
#3270=ORIENTED_EDGE('',*,*,#2686,.F.);
#3271=ORIENTED_EDGE('',*,*,#2687,.T.);
#3272=ORIENTED_EDGE('',*,*,#2686,.T.);
#3273=ORIENTED_EDGE('',*,*,#2688,.F.);
#3274=ORIENTED_EDGE('',*,*,#2678,.F.);
#3275=ORIENTED_EDGE('',*,*,#2688,.T.);
#3276=ORIENTED_EDGE('',*,*,#2685,.T.);
#3277=ORIENTED_EDGE('',*,*,#2682,.T.);
#3278=ORIENTED_EDGE('',*,*,#2679,.T.);
#3279=ORIENTED_EDGE('',*,*,#2667,.T.);
#3280=ORIENTED_EDGE('',*,*,#2670,.T.);
#3281=ORIENTED_EDGE('',*,*,#2673,.T.);
#3282=ORIENTED_EDGE('',*,*,#2676,.T.);
#3283=ORIENTED_EDGE('',*,*,#2687,.F.);
#3284=ORIENTED_EDGE('',*,*,#2677,.F.);
#3285=ORIENTED_EDGE('',*,*,#2681,.F.);
#3286=ORIENTED_EDGE('',*,*,#2684,.F.);
#3287=ORIENTED_EDGE('',*,*,#2665,.T.);
#3288=ORIENTED_EDGE('',*,*,#2668,.T.);
#3289=ORIENTED_EDGE('',*,*,#2671,.T.);
#3290=ORIENTED_EDGE('',*,*,#2674,.T.);
#3291=ORIENTED_EDGE('',*,*,#2689,.T.);
#3292=ORIENTED_EDGE('',*,*,#2690,.T.);
#3293=ORIENTED_EDGE('',*,*,#2691,.F.);
#3294=ORIENTED_EDGE('',*,*,#2692,.F.);
#3295=ORIENTED_EDGE('',*,*,#2693,.T.);
#3296=ORIENTED_EDGE('',*,*,#2692,.T.);
#3297=ORIENTED_EDGE('',*,*,#2694,.F.);
#3298=ORIENTED_EDGE('',*,*,#2695,.F.);
#3299=ORIENTED_EDGE('',*,*,#2696,.T.);
#3300=ORIENTED_EDGE('',*,*,#2695,.T.);
#3301=ORIENTED_EDGE('',*,*,#2697,.F.);
#3302=ORIENTED_EDGE('',*,*,#2698,.F.);
#3303=ORIENTED_EDGE('',*,*,#2699,.T.);
#3304=ORIENTED_EDGE('',*,*,#2698,.T.);
#3305=ORIENTED_EDGE('',*,*,#2700,.F.);
#3306=ORIENTED_EDGE('',*,*,#2690,.F.);
#3307=ORIENTED_EDGE('',*,*,#2700,.T.);
#3308=ORIENTED_EDGE('',*,*,#2697,.T.);
#3309=ORIENTED_EDGE('',*,*,#2694,.T.);
#3310=ORIENTED_EDGE('',*,*,#2691,.T.);
#3311=ORIENTED_EDGE('',*,*,#2699,.F.);
#3312=ORIENTED_EDGE('',*,*,#2689,.F.);
#3313=ORIENTED_EDGE('',*,*,#2693,.F.);
#3314=ORIENTED_EDGE('',*,*,#2696,.F.);
#3315=ORIENTED_EDGE('',*,*,#2701,.T.);
#3316=ORIENTED_EDGE('',*,*,#2702,.T.);
#3317=ORIENTED_EDGE('',*,*,#2703,.F.);
#3318=ORIENTED_EDGE('',*,*,#2704,.F.);
#3319=ORIENTED_EDGE('',*,*,#2705,.T.);
#3320=ORIENTED_EDGE('',*,*,#2704,.T.);
#3321=ORIENTED_EDGE('',*,*,#2706,.F.);
#3322=ORIENTED_EDGE('',*,*,#2707,.F.);
#3323=ORIENTED_EDGE('',*,*,#2708,.T.);
#3324=ORIENTED_EDGE('',*,*,#2707,.T.);
#3325=ORIENTED_EDGE('',*,*,#2709,.F.);
#3326=ORIENTED_EDGE('',*,*,#2710,.F.);
#3327=ORIENTED_EDGE('',*,*,#2711,.T.);
#3328=ORIENTED_EDGE('',*,*,#2710,.T.);
#3329=ORIENTED_EDGE('',*,*,#2712,.F.);
#3330=ORIENTED_EDGE('',*,*,#2702,.F.);
#3331=ORIENTED_EDGE('',*,*,#2712,.T.);
#3332=ORIENTED_EDGE('',*,*,#2709,.T.);
#3333=ORIENTED_EDGE('',*,*,#2706,.T.);
#3334=ORIENTED_EDGE('',*,*,#2703,.T.);
#3335=ORIENTED_EDGE('',*,*,#2711,.F.);
#3336=ORIENTED_EDGE('',*,*,#2701,.F.);
#3337=ORIENTED_EDGE('',*,*,#2705,.F.);
#3338=ORIENTED_EDGE('',*,*,#2708,.F.);
#3339=ORIENTED_EDGE('',*,*,#2713,.F.);
#3340=ORIENTED_EDGE('',*,*,#2714,.T.);
#3341=ORIENTED_EDGE('',*,*,#2715,.F.);
#3342=ORIENTED_EDGE('',*,*,#2714,.F.);
#3343=ORIENTED_EDGE('',*,*,#2716,.F.);
#3344=ORIENTED_EDGE('',*,*,#2717,.T.);
#3345=ORIENTED_EDGE('',*,*,#2718,.F.);
#3346=ORIENTED_EDGE('',*,*,#2717,.F.);
#3347=ORIENTED_EDGE('',*,*,#2719,.F.);
#3348=ORIENTED_EDGE('',*,*,#2720,.T.);
#3349=ORIENTED_EDGE('',*,*,#2721,.F.);
#3350=ORIENTED_EDGE('',*,*,#2720,.F.);
#3351=ORIENTED_EDGE('',*,*,#2722,.F.);
#3352=ORIENTED_EDGE('',*,*,#2723,.T.);
#3353=ORIENTED_EDGE('',*,*,#2724,.F.);
#3354=ORIENTED_EDGE('',*,*,#2723,.F.);
#3355=ORIENTED_EDGE('',*,*,#2725,.T.);
#3356=ORIENTED_EDGE('',*,*,#2726,.T.);
#3357=ORIENTED_EDGE('',*,*,#2727,.F.);
#3358=ORIENTED_EDGE('',*,*,#2728,.F.);
#3359=ORIENTED_EDGE('',*,*,#2729,.T.);
#3360=ORIENTED_EDGE('',*,*,#2728,.T.);
#3361=ORIENTED_EDGE('',*,*,#2730,.F.);
#3362=ORIENTED_EDGE('',*,*,#2731,.F.);
#3363=ORIENTED_EDGE('',*,*,#2732,.T.);
#3364=ORIENTED_EDGE('',*,*,#2731,.T.);
#3365=ORIENTED_EDGE('',*,*,#2733,.F.);
#3366=ORIENTED_EDGE('',*,*,#2734,.F.);
#3367=ORIENTED_EDGE('',*,*,#2735,.T.);
#3368=ORIENTED_EDGE('',*,*,#2734,.T.);
#3369=ORIENTED_EDGE('',*,*,#2736,.F.);
#3370=ORIENTED_EDGE('',*,*,#2726,.F.);
#3371=ORIENTED_EDGE('',*,*,#2736,.T.);
#3372=ORIENTED_EDGE('',*,*,#2733,.T.);
#3373=ORIENTED_EDGE('',*,*,#2730,.T.);
#3374=ORIENTED_EDGE('',*,*,#2727,.T.);
#3375=ORIENTED_EDGE('',*,*,#2715,.T.);
#3376=ORIENTED_EDGE('',*,*,#2718,.T.);
#3377=ORIENTED_EDGE('',*,*,#2721,.T.);
#3378=ORIENTED_EDGE('',*,*,#2724,.T.);
#3379=ORIENTED_EDGE('',*,*,#2735,.F.);
#3380=ORIENTED_EDGE('',*,*,#2725,.F.);
#3381=ORIENTED_EDGE('',*,*,#2729,.F.);
#3382=ORIENTED_EDGE('',*,*,#2732,.F.);
#3383=ORIENTED_EDGE('',*,*,#2713,.T.);
#3384=ORIENTED_EDGE('',*,*,#2716,.T.);
#3385=ORIENTED_EDGE('',*,*,#2719,.T.);
#3386=ORIENTED_EDGE('',*,*,#2722,.T.);
#3387=ORIENTED_EDGE('',*,*,#2737,.F.);
#3388=ORIENTED_EDGE('',*,*,#2738,.T.);
#3389=ORIENTED_EDGE('',*,*,#2739,.T.);
#3390=ORIENTED_EDGE('',*,*,#2738,.F.);
#3391=ORIENTED_EDGE('',*,*,#2740,.F.);
#3392=ORIENTED_EDGE('',*,*,#2741,.T.);
#3393=ORIENTED_EDGE('',*,*,#2742,.T.);
#3394=ORIENTED_EDGE('',*,*,#2741,.F.);
#3395=ORIENTED_EDGE('',*,*,#2740,.T.);
#3396=ORIENTED_EDGE('',*,*,#2737,.T.);
#3397=ORIENTED_EDGE('',*,*,#2742,.F.);
#3398=ORIENTED_EDGE('',*,*,#2739,.F.);
#3399=ORIENTED_EDGE('',*,*,#2743,.F.);
#3400=ORIENTED_EDGE('',*,*,#2744,.T.);
#3401=ORIENTED_EDGE('',*,*,#2745,.T.);
#3402=ORIENTED_EDGE('',*,*,#2744,.F.);
#3403=ORIENTED_EDGE('',*,*,#2746,.F.);
#3404=ORIENTED_EDGE('',*,*,#2747,.T.);
#3405=ORIENTED_EDGE('',*,*,#2748,.T.);
#3406=ORIENTED_EDGE('',*,*,#2747,.F.);
#3407=ORIENTED_EDGE('',*,*,#2746,.T.);
#3408=ORIENTED_EDGE('',*,*,#2743,.T.);
#3409=ORIENTED_EDGE('',*,*,#2748,.F.);
#3410=ORIENTED_EDGE('',*,*,#2745,.F.);
#3411=ORIENTED_EDGE('',*,*,#2749,.F.);
#3412=ORIENTED_EDGE('',*,*,#2750,.T.);
#3413=ORIENTED_EDGE('',*,*,#2751,.F.);
#3414=ORIENTED_EDGE('',*,*,#2750,.F.);
#3415=ORIENTED_EDGE('',*,*,#2752,.F.);
#3416=ORIENTED_EDGE('',*,*,#2753,.T.);
#3417=ORIENTED_EDGE('',*,*,#2754,.F.);
#3418=ORIENTED_EDGE('',*,*,#2753,.F.);
#3419=ORIENTED_EDGE('',*,*,#2755,.F.);
#3420=ORIENTED_EDGE('',*,*,#2756,.T.);
#3421=ORIENTED_EDGE('',*,*,#2757,.F.);
#3422=ORIENTED_EDGE('',*,*,#2756,.F.);
#3423=ORIENTED_EDGE('',*,*,#2758,.F.);
#3424=ORIENTED_EDGE('',*,*,#2759,.T.);
#3425=ORIENTED_EDGE('',*,*,#2760,.F.);
#3426=ORIENTED_EDGE('',*,*,#2759,.F.);
#3427=ORIENTED_EDGE('',*,*,#2761,.T.);
#3428=ORIENTED_EDGE('',*,*,#2762,.T.);
#3429=ORIENTED_EDGE('',*,*,#2763,.F.);
#3430=ORIENTED_EDGE('',*,*,#2764,.F.);
#3431=ORIENTED_EDGE('',*,*,#2765,.T.);
#3432=ORIENTED_EDGE('',*,*,#2764,.T.);
#3433=ORIENTED_EDGE('',*,*,#2766,.F.);
#3434=ORIENTED_EDGE('',*,*,#2767,.F.);
#3435=ORIENTED_EDGE('',*,*,#2768,.T.);
#3436=ORIENTED_EDGE('',*,*,#2767,.T.);
#3437=ORIENTED_EDGE('',*,*,#2769,.F.);
#3438=ORIENTED_EDGE('',*,*,#2770,.F.);
#3439=ORIENTED_EDGE('',*,*,#2771,.T.);
#3440=ORIENTED_EDGE('',*,*,#2770,.T.);
#3441=ORIENTED_EDGE('',*,*,#2772,.F.);
#3442=ORIENTED_EDGE('',*,*,#2762,.F.);
#3443=ORIENTED_EDGE('',*,*,#2772,.T.);
#3444=ORIENTED_EDGE('',*,*,#2769,.T.);
#3445=ORIENTED_EDGE('',*,*,#2766,.T.);
#3446=ORIENTED_EDGE('',*,*,#2763,.T.);
#3447=ORIENTED_EDGE('',*,*,#2751,.T.);
#3448=ORIENTED_EDGE('',*,*,#2754,.T.);
#3449=ORIENTED_EDGE('',*,*,#2757,.T.);
#3450=ORIENTED_EDGE('',*,*,#2760,.T.);
#3451=ORIENTED_EDGE('',*,*,#2771,.F.);
#3452=ORIENTED_EDGE('',*,*,#2761,.F.);
#3453=ORIENTED_EDGE('',*,*,#2765,.F.);
#3454=ORIENTED_EDGE('',*,*,#2768,.F.);
#3455=ORIENTED_EDGE('',*,*,#2749,.T.);
#3456=ORIENTED_EDGE('',*,*,#2752,.T.);
#3457=ORIENTED_EDGE('',*,*,#2755,.T.);
#3458=ORIENTED_EDGE('',*,*,#2758,.T.);
#3459=ORIENTED_EDGE('',*,*,#2773,.F.);
#3460=ORIENTED_EDGE('',*,*,#2774,.T.);
#3461=ORIENTED_EDGE('',*,*,#2775,.T.);
#3462=ORIENTED_EDGE('',*,*,#2774,.F.);
#3463=ORIENTED_EDGE('',*,*,#2776,.F.);
#3464=ORIENTED_EDGE('',*,*,#2777,.T.);
#3465=ORIENTED_EDGE('',*,*,#2778,.T.);
#3466=ORIENTED_EDGE('',*,*,#2777,.F.);
#3467=ORIENTED_EDGE('',*,*,#2776,.T.);
#3468=ORIENTED_EDGE('',*,*,#2773,.T.);
#3469=ORIENTED_EDGE('',*,*,#2778,.F.);
#3470=ORIENTED_EDGE('',*,*,#2775,.F.);
#3471=ORIENTED_EDGE('',*,*,#2779,.F.);
#3472=ORIENTED_EDGE('',*,*,#2780,.T.);
#3473=ORIENTED_EDGE('',*,*,#2781,.T.);
#3474=ORIENTED_EDGE('',*,*,#2780,.F.);
#3475=ORIENTED_EDGE('',*,*,#2782,.F.);
#3476=ORIENTED_EDGE('',*,*,#2783,.T.);
#3477=ORIENTED_EDGE('',*,*,#2784,.T.);
#3478=ORIENTED_EDGE('',*,*,#2783,.F.);
#3479=ORIENTED_EDGE('',*,*,#2782,.T.);
#3480=ORIENTED_EDGE('',*,*,#2779,.T.);
#3481=ORIENTED_EDGE('',*,*,#2784,.F.);
#3482=ORIENTED_EDGE('',*,*,#2781,.F.);
#3483=ORIENTED_EDGE('',*,*,#2785,.F.);
#3484=ORIENTED_EDGE('',*,*,#2786,.T.);
#3485=ORIENTED_EDGE('',*,*,#2787,.F.);
#3486=ORIENTED_EDGE('',*,*,#2786,.F.);
#3487=ORIENTED_EDGE('',*,*,#2788,.F.);
#3488=ORIENTED_EDGE('',*,*,#2789,.T.);
#3489=ORIENTED_EDGE('',*,*,#2790,.F.);
#3490=ORIENTED_EDGE('',*,*,#2789,.F.);
#3491=ORIENTED_EDGE('',*,*,#2791,.T.);
#3492=ORIENTED_EDGE('',*,*,#2791,.F.);
#3493=ORIENTED_EDGE('',*,*,#2788,.T.);
#3494=ORIENTED_EDGE('',*,*,#2787,.T.);
#3495=ORIENTED_EDGE('',*,*,#2792,.F.);
#3496=ORIENTED_EDGE('',*,*,#2793,.T.);
#3497=ORIENTED_EDGE('',*,*,#2794,.F.);
#3498=ORIENTED_EDGE('',*,*,#2795,.F.);
#3499=ORIENTED_EDGE('',*,*,#2796,.F.);
#3500=ORIENTED_EDGE('',*,*,#2797,.T.);
#3501=ORIENTED_EDGE('',*,*,#2798,.F.);
#3502=ORIENTED_EDGE('',*,*,#2799,.F.);
#3503=ORIENTED_EDGE('',*,*,#2800,.T.);
#3504=ORIENTED_EDGE('',*,*,#2801,.F.);
#3505=ORIENTED_EDGE('',*,*,#2800,.F.);
#3506=ORIENTED_EDGE('',*,*,#2802,.F.);
#3507=ORIENTED_EDGE('',*,*,#2793,.F.);
#3508=ORIENTED_EDGE('',*,*,#2803,.F.);
#3509=ORIENTED_EDGE('',*,*,#2804,.T.);
#3510=ORIENTED_EDGE('',*,*,#2805,.F.);
#3511=ORIENTED_EDGE('',*,*,#2806,.F.);
#3512=ORIENTED_EDGE('',*,*,#2797,.F.);
#3513=ORIENTED_EDGE('',*,*,#2807,.F.);
#3514=ORIENTED_EDGE('',*,*,#2804,.F.);
#3515=ORIENTED_EDGE('',*,*,#2808,.T.);
#3516=ORIENTED_EDGE('',*,*,#2809,.T.);
#3517=ORIENTED_EDGE('',*,*,#2810,.T.);
#3518=ORIENTED_EDGE('',*,*,#2811,.T.);
#3519=ORIENTED_EDGE('',*,*,#2812,.T.);
#3520=ORIENTED_EDGE('',*,*,#2813,.T.);
#3521=ORIENTED_EDGE('',*,*,#2795,.T.);
#3522=ORIENTED_EDGE('',*,*,#2806,.T.);
#3523=ORIENTED_EDGE('',*,*,#2803,.T.);
#3524=ORIENTED_EDGE('',*,*,#2814,.T.);
#3525=ORIENTED_EDGE('',*,*,#2815,.T.);
#3526=ORIENTED_EDGE('',*,*,#2816,.T.);
#3527=ORIENTED_EDGE('',*,*,#2798,.T.);
#3528=ORIENTED_EDGE('',*,*,#2801,.T.);
#3529=ORIENTED_EDGE('',*,*,#2792,.T.);
#3530=ORIENTED_EDGE('',*,*,#2817,.T.);
#3531=ORIENTED_EDGE('',*,*,#2818,.T.);
#3532=ORIENTED_EDGE('',*,*,#2819,.T.);
#3533=ORIENTED_EDGE('',*,*,#2796,.T.);
#3534=ORIENTED_EDGE('',*,*,#2819,.F.);
#3535=ORIENTED_EDGE('',*,*,#2820,.F.);
#3536=ORIENTED_EDGE('',*,*,#2817,.F.);
#3537=ORIENTED_EDGE('',*,*,#2794,.T.);
#3538=ORIENTED_EDGE('',*,*,#2802,.T.);
#3539=ORIENTED_EDGE('',*,*,#2799,.T.);
#3540=ORIENTED_EDGE('',*,*,#2816,.F.);
#3541=ORIENTED_EDGE('',*,*,#2821,.F.);
#3542=ORIENTED_EDGE('',*,*,#2814,.F.);
#3543=ORIENTED_EDGE('',*,*,#2805,.T.);
#3544=ORIENTED_EDGE('',*,*,#2807,.T.);
#3545=ORIENTED_EDGE('',*,*,#2815,.F.);
#3546=ORIENTED_EDGE('',*,*,#2821,.T.);
#3547=ORIENTED_EDGE('',*,*,#2785,.T.);
#3548=ORIENTED_EDGE('',*,*,#2818,.F.);
#3549=ORIENTED_EDGE('',*,*,#2820,.T.);
#3550=ORIENTED_EDGE('',*,*,#2790,.T.);
#3551=ORIENTED_EDGE('',*,*,#2822,.F.);
#3552=ORIENTED_EDGE('',*,*,#2823,.T.);
#3553=ORIENTED_EDGE('',*,*,#2824,.T.);
#3554=ORIENTED_EDGE('',*,*,#2825,.F.);
#3555=ORIENTED_EDGE('',*,*,#2826,.F.);
#3556=ORIENTED_EDGE('',*,*,#2827,.T.);
#3557=ORIENTED_EDGE('',*,*,#2828,.T.);
#3558=ORIENTED_EDGE('',*,*,#2823,.F.);
#3559=ORIENTED_EDGE('',*,*,#2829,.F.);
#3560=ORIENTED_EDGE('',*,*,#2830,.T.);
#3561=ORIENTED_EDGE('',*,*,#2831,.T.);
#3562=ORIENTED_EDGE('',*,*,#2827,.F.);
#3563=ORIENTED_EDGE('',*,*,#2832,.F.);
#3564=ORIENTED_EDGE('',*,*,#2825,.T.);
#3565=ORIENTED_EDGE('',*,*,#2833,.T.);
#3566=ORIENTED_EDGE('',*,*,#2830,.F.);
#3567=ORIENTED_EDGE('',*,*,#2833,.F.);
#3568=ORIENTED_EDGE('',*,*,#2824,.F.);
#3569=ORIENTED_EDGE('',*,*,#2828,.F.);
#3570=ORIENTED_EDGE('',*,*,#2831,.F.);
#3571=ORIENTED_EDGE('',*,*,#2834,.F.);
#3572=ORIENTED_EDGE('',*,*,#2835,.T.);
#3573=ORIENTED_EDGE('',*,*,#2813,.F.);
#3574=ORIENTED_EDGE('',*,*,#2835,.F.);
#3575=ORIENTED_EDGE('',*,*,#2836,.F.);
#3576=ORIENTED_EDGE('',*,*,#2837,.T.);
#3577=ORIENTED_EDGE('',*,*,#2812,.F.);
#3578=ORIENTED_EDGE('',*,*,#2837,.F.);
#3579=ORIENTED_EDGE('',*,*,#2838,.T.);
#3580=ORIENTED_EDGE('',*,*,#2839,.T.);
#3581=ORIENTED_EDGE('',*,*,#2811,.F.);
#3582=ORIENTED_EDGE('',*,*,#2840,.F.);
#3583=ORIENTED_EDGE('',*,*,#2841,.T.);
#3584=ORIENTED_EDGE('',*,*,#2840,.T.);
#3585=ORIENTED_EDGE('',*,*,#2810,.F.);
#3586=ORIENTED_EDGE('',*,*,#2842,.F.);
#3587=ORIENTED_EDGE('',*,*,#2843,.T.);
#3588=ORIENTED_EDGE('',*,*,#2842,.T.);
#3589=ORIENTED_EDGE('',*,*,#2809,.F.);
#3590=ORIENTED_EDGE('',*,*,#2844,.F.);
#3591=ORIENTED_EDGE('',*,*,#2845,.T.);
#3592=ORIENTED_EDGE('',*,*,#2844,.T.);
#3593=ORIENTED_EDGE('',*,*,#2808,.F.);
#3594=ORIENTED_EDGE('',*,*,#2839,.F.);
#3595=ORIENTED_EDGE('',*,*,#2845,.F.);
#3596=ORIENTED_EDGE('',*,*,#2838,.F.);
#3597=ORIENTED_EDGE('',*,*,#2841,.F.);
#3598=ORIENTED_EDGE('',*,*,#2843,.F.);
#3599=ORIENTED_EDGE('',*,*,#2822,.T.);
#3600=ORIENTED_EDGE('',*,*,#2832,.T.);
#3601=ORIENTED_EDGE('',*,*,#2829,.T.);
#3602=ORIENTED_EDGE('',*,*,#2826,.T.);
#3603=ORIENTED_EDGE('',*,*,#2834,.T.);
#3604=ORIENTED_EDGE('',*,*,#2836,.T.);
#3605=ORIENTED_EDGE('',*,*,#2846,.T.);
#3606=ORIENTED_EDGE('',*,*,#2847,.T.);
#3607=ORIENTED_EDGE('',*,*,#2848,.F.);
#3608=ORIENTED_EDGE('',*,*,#2847,.F.);
#3609=ORIENTED_EDGE('',*,*,#2849,.F.);
#3610=ORIENTED_EDGE('',*,*,#2848,.T.);
#3611=ORIENTED_EDGE('',*,*,#2850,.T.);
#3612=ORIENTED_EDGE('',*,*,#2850,.F.);
#3613=ORIENTED_EDGE('',*,*,#2849,.T.);
#3614=ORIENTED_EDGE('',*,*,#2851,.F.);
#3615=ORIENTED_EDGE('',*,*,#2851,.T.);
#3616=ORIENTED_EDGE('',*,*,#2846,.F.);
#3617=ORIENTED_EDGE('',*,*,#2852,.F.);
#3618=ORIENTED_EDGE('',*,*,#2853,.F.);
#3619=ORIENTED_EDGE('',*,*,#2854,.F.);
#3620=ORIENTED_EDGE('',*,*,#2855,.T.);
#3621=ORIENTED_EDGE('',*,*,#2856,.F.);
#3622=ORIENTED_EDGE('',*,*,#2855,.F.);
#3623=ORIENTED_EDGE('',*,*,#2857,.F.);
#3624=ORIENTED_EDGE('',*,*,#2858,.T.);
#3625=ORIENTED_EDGE('',*,*,#2859,.F.);
#3626=ORIENTED_EDGE('',*,*,#2860,.F.);
#3627=ORIENTED_EDGE('',*,*,#2861,.F.);
#3628=ORIENTED_EDGE('',*,*,#2858,.F.);
#3629=ORIENTED_EDGE('',*,*,#2862,.F.);
#3630=ORIENTED_EDGE('',*,*,#2863,.T.);
#3631=ORIENTED_EDGE('',*,*,#2864,.T.);
#3632=ORIENTED_EDGE('',*,*,#2863,.F.);
#3633=ORIENTED_EDGE('',*,*,#2853,.T.);
#3634=ORIENTED_EDGE('',*,*,#2852,.T.);
#3635=ORIENTED_EDGE('',*,*,#2854,.T.);
#3636=ORIENTED_EDGE('',*,*,#2860,.T.);
#3637=ORIENTED_EDGE('',*,*,#2859,.T.);
#3638=ORIENTED_EDGE('',*,*,#2861,.T.);
#3639=ORIENTED_EDGE('',*,*,#2865,.T.);
#3640=ORIENTED_EDGE('',*,*,#2866,.T.);
#3641=ORIENTED_EDGE('',*,*,#2867,.T.);
#3642=ORIENTED_EDGE('',*,*,#2868,.T.);
#3643=ORIENTED_EDGE('',*,*,#2869,.T.);
#3644=ORIENTED_EDGE('',*,*,#2870,.T.);
#3645=ORIENTED_EDGE('',*,*,#2871,.T.);
#3646=ORIENTED_EDGE('',*,*,#2872,.T.);
#3647=ORIENTED_EDGE('',*,*,#2873,.T.);
#3648=ORIENTED_EDGE('',*,*,#2874,.T.);
#3649=ORIENTED_EDGE('',*,*,#2875,.T.);
#3650=ORIENTED_EDGE('',*,*,#2876,.T.);
#3651=ORIENTED_EDGE('',*,*,#2866,.F.);
#3652=ORIENTED_EDGE('',*,*,#2865,.F.);
#3653=ORIENTED_EDGE('',*,*,#2867,.F.);
#3654=ORIENTED_EDGE('',*,*,#2877,.T.);
#3655=ORIENTED_EDGE('',*,*,#2878,.F.);
#3656=ORIENTED_EDGE('',*,*,#2877,.F.);
#3657=ORIENTED_EDGE('',*,*,#2879,.F.);
#3658=ORIENTED_EDGE('',*,*,#2880,.T.);
#3659=ORIENTED_EDGE('',*,*,#2869,.F.);
#3660=ORIENTED_EDGE('',*,*,#2868,.F.);
#3661=ORIENTED_EDGE('',*,*,#2870,.F.);
#3662=ORIENTED_EDGE('',*,*,#2880,.F.);
#3663=ORIENTED_EDGE('',*,*,#2872,.F.);
#3664=ORIENTED_EDGE('',*,*,#2871,.F.);
#3665=ORIENTED_EDGE('',*,*,#2873,.F.);
#3666=ORIENTED_EDGE('',*,*,#2881,.T.);
#3667=ORIENTED_EDGE('',*,*,#2882,.F.);
#3668=ORIENTED_EDGE('',*,*,#2881,.F.);
#3669=ORIENTED_EDGE('',*,*,#2883,.F.);
#3670=ORIENTED_EDGE('',*,*,#2884,.T.);
#3671=ORIENTED_EDGE('',*,*,#2875,.F.);
#3672=ORIENTED_EDGE('',*,*,#2874,.F.);
#3673=ORIENTED_EDGE('',*,*,#2876,.F.);
#3674=ORIENTED_EDGE('',*,*,#2884,.F.);
#3675=ORIENTED_EDGE('',*,*,#2864,.F.);
#3676=ORIENTED_EDGE('',*,*,#2885,.T.);
#3677=ORIENTED_EDGE('',*,*,#2886,.F.);
#3678=ORIENTED_EDGE('',*,*,#2862,.T.);
#3679=ORIENTED_EDGE('',*,*,#2887,.F.);
#3680=ORIENTED_EDGE('',*,*,#2888,.T.);
#3681=ORIENTED_EDGE('',*,*,#2886,.T.);
#3682=ORIENTED_EDGE('',*,*,#2888,.F.);
#3683=ORIENTED_EDGE('',*,*,#2887,.T.);
#3684=ORIENTED_EDGE('',*,*,#2889,.F.);
#3685=ORIENTED_EDGE('',*,*,#2889,.T.);
#3686=ORIENTED_EDGE('',*,*,#2890,.T.);
#3687=ORIENTED_EDGE('',*,*,#2885,.F.);
#3688=ORIENTED_EDGE('',*,*,#2890,.F.);
#3689=ORIENTED_EDGE('',*,*,#2857,.T.);
#3690=ORIENTED_EDGE('',*,*,#2856,.T.);
#3691=ORIENTED_EDGE('',*,*,#2879,.T.);
#3692=ORIENTED_EDGE('',*,*,#2878,.T.);
#3693=ORIENTED_EDGE('',*,*,#2883,.T.);
#3694=ORIENTED_EDGE('',*,*,#2882,.T.);
#3695=ORIENTED_EDGE('',*,*,#2891,.F.);
#3696=ORIENTED_EDGE('',*,*,#2892,.T.);
#3697=ORIENTED_EDGE('',*,*,#2893,.T.);
#3698=ORIENTED_EDGE('',*,*,#2892,.F.);
#3699=ORIENTED_EDGE('',*,*,#2894,.F.);
#3700=ORIENTED_EDGE('',*,*,#2895,.T.);
#3701=ORIENTED_EDGE('',*,*,#2896,.T.);
#3702=ORIENTED_EDGE('',*,*,#2895,.F.);
#3703=ORIENTED_EDGE('',*,*,#2894,.T.);
#3704=ORIENTED_EDGE('',*,*,#2891,.T.);
#3705=ORIENTED_EDGE('',*,*,#2896,.F.);
#3706=ORIENTED_EDGE('',*,*,#2893,.F.);
#3707=ORIENTED_EDGE('',*,*,#2897,.T.);
#3708=ORIENTED_EDGE('',*,*,#2898,.T.);
#3709=ORIENTED_EDGE('',*,*,#2899,.T.);
#3710=ORIENTED_EDGE('',*,*,#2900,.F.);
#3711=ORIENTED_EDGE('',*,*,#2901,.T.);
#3712=ORIENTED_EDGE('',*,*,#2902,.T.);
#3713=ORIENTED_EDGE('',*,*,#2903,.T.);
#3714=ORIENTED_EDGE('',*,*,#2898,.F.);
#3715=ORIENTED_EDGE('',*,*,#2904,.T.);
#3716=ORIENTED_EDGE('',*,*,#2905,.T.);
#3717=ORIENTED_EDGE('',*,*,#2906,.T.);
#3718=ORIENTED_EDGE('',*,*,#2902,.F.);
#3719=ORIENTED_EDGE('',*,*,#2907,.T.);
#3720=ORIENTED_EDGE('',*,*,#2908,.T.);
#3721=ORIENTED_EDGE('',*,*,#2909,.T.);
#3722=ORIENTED_EDGE('',*,*,#2905,.F.);
#3723=ORIENTED_EDGE('',*,*,#2910,.T.);
#3724=ORIENTED_EDGE('',*,*,#2911,.T.);
#3725=ORIENTED_EDGE('',*,*,#2912,.T.);
#3726=ORIENTED_EDGE('',*,*,#2908,.F.);
#3727=ORIENTED_EDGE('',*,*,#2913,.T.);
#3728=ORIENTED_EDGE('',*,*,#2900,.T.);
#3729=ORIENTED_EDGE('',*,*,#2914,.T.);
#3730=ORIENTED_EDGE('',*,*,#2911,.F.);
#3731=ORIENTED_EDGE('',*,*,#2913,.F.);
#3732=ORIENTED_EDGE('',*,*,#2910,.F.);
#3733=ORIENTED_EDGE('',*,*,#2907,.F.);
#3734=ORIENTED_EDGE('',*,*,#2904,.F.);
#3735=ORIENTED_EDGE('',*,*,#2901,.F.);
#3736=ORIENTED_EDGE('',*,*,#2897,.F.);
#3737=ORIENTED_EDGE('',*,*,#2914,.F.);
#3738=ORIENTED_EDGE('',*,*,#2899,.F.);
#3739=ORIENTED_EDGE('',*,*,#2903,.F.);
#3740=ORIENTED_EDGE('',*,*,#2906,.F.);
#3741=ORIENTED_EDGE('',*,*,#2909,.F.);
#3742=ORIENTED_EDGE('',*,*,#2912,.F.);
#3743=ORIENTED_EDGE('',*,*,#2915,.F.);
#3744=ORIENTED_EDGE('',*,*,#2916,.F.);
#3745=ORIENTED_EDGE('',*,*,#2917,.F.);
#3746=ORIENTED_EDGE('',*,*,#2918,.T.);
#3747=ORIENTED_EDGE('',*,*,#2916,.T.);
#3748=ORIENTED_EDGE('',*,*,#2918,.F.);
#3749=ORIENTED_EDGE('',*,*,#2919,.F.);
#3750=ORIENTED_EDGE('',*,*,#2920,.T.);
#3751=ORIENTED_EDGE('',*,*,#2917,.T.);
#3752=ORIENTED_EDGE('',*,*,#2920,.F.);
#3753=ORIENTED_EDGE('',*,*,#2921,.F.);
#3754=ORIENTED_EDGE('',*,*,#2922,.T.);
#3755=ORIENTED_EDGE('',*,*,#2919,.T.);
#3756=ORIENTED_EDGE('',*,*,#2922,.F.);
#3757=ORIENTED_EDGE('',*,*,#2921,.T.);
#3758=ORIENTED_EDGE('',*,*,#2923,.F.);
#3759=ORIENTED_EDGE('',*,*,#2924,.F.);
#3760=ORIENTED_EDGE('',*,*,#2925,.T.);
#3761=ORIENTED_EDGE('',*,*,#2923,.T.);
#3762=ORIENTED_EDGE('',*,*,#2925,.F.);
#3763=ORIENTED_EDGE('',*,*,#2915,.T.);
#3764=ORIENTED_EDGE('',*,*,#2926,.T.);
#3765=ORIENTED_EDGE('',*,*,#2924,.T.);
#3766=ORIENTED_EDGE('',*,*,#2926,.F.);
#3767=ORIENTED_EDGE('',*,*,#2927,.F.);
#3768=ORIENTED_EDGE('',*,*,#2928,.T.);
#3769=ORIENTED_EDGE('',*,*,#2929,.T.);
#3770=ORIENTED_EDGE('',*,*,#2928,.F.);
#3771=ORIENTED_EDGE('',*,*,#2929,.F.);
#3772=ORIENTED_EDGE('',*,*,#2930,.F.);
#3773=ORIENTED_EDGE('',*,*,#2931,.T.);
#3774=ORIENTED_EDGE('',*,*,#2932,.F.);
#3775=ORIENTED_EDGE('',*,*,#2933,.T.);
#3776=ORIENTED_EDGE('',*,*,#2934,.F.);
#3777=ORIENTED_EDGE('',*,*,#2933,.F.);
#3778=ORIENTED_EDGE('',*,*,#2935,.F.);
#3779=ORIENTED_EDGE('',*,*,#2936,.F.);
#3780=ORIENTED_EDGE('',*,*,#2937,.F.);
#3781=ORIENTED_EDGE('',*,*,#2936,.T.);
#3782=ORIENTED_EDGE('',*,*,#2938,.T.);
#3783=ORIENTED_EDGE('',*,*,#2939,.T.);
#3784=ORIENTED_EDGE('',*,*,#2935,.T.);
#3785=ORIENTED_EDGE('',*,*,#2932,.T.);
#3786=ORIENTED_EDGE('',*,*,#2940,.T.);
#3787=ORIENTED_EDGE('',*,*,#2938,.F.);
#3788=ORIENTED_EDGE('',*,*,#2941,.F.);
#3789=ORIENTED_EDGE('',*,*,#2939,.F.);
#3790=ORIENTED_EDGE('',*,*,#2940,.F.);
#3791=ORIENTED_EDGE('',*,*,#2931,.F.);
#3792=ORIENTED_EDGE('',*,*,#2942,.F.);
#3793=ORIENTED_EDGE('',*,*,#2943,.T.);
#3794=ORIENTED_EDGE('',*,*,#2944,.T.);
#3795=ORIENTED_EDGE('',*,*,#2943,.F.);
#3796=ORIENTED_EDGE('',*,*,#2937,.T.);
#3797=ORIENTED_EDGE('',*,*,#2941,.T.);
#3798=ORIENTED_EDGE('',*,*,#2930,.T.);
#3799=ORIENTED_EDGE('',*,*,#2934,.T.);
#3800=ORIENTED_EDGE('',*,*,#2942,.T.);
#3801=ORIENTED_EDGE('',*,*,#2944,.F.);
#3802=ORIENTED_EDGE('',*,*,#2927,.T.);
#3803=ORIENTED_EDGE('',*,*,#2945,.F.);
#3804=ORIENTED_EDGE('',*,*,#2946,.T.);
#3805=ORIENTED_EDGE('',*,*,#2947,.F.);
#3806=ORIENTED_EDGE('',*,*,#2946,.F.);
#3807=ORIENTED_EDGE('',*,*,#2948,.F.);
#3808=ORIENTED_EDGE('',*,*,#2949,.T.);
#3809=ORIENTED_EDGE('',*,*,#2950,.F.);
#3810=ORIENTED_EDGE('',*,*,#2949,.F.);
#3811=ORIENTED_EDGE('',*,*,#2951,.F.);
#3812=ORIENTED_EDGE('',*,*,#2952,.T.);
#3813=ORIENTED_EDGE('',*,*,#2953,.F.);
#3814=ORIENTED_EDGE('',*,*,#2952,.F.);
#3815=ORIENTED_EDGE('',*,*,#2954,.F.);
#3816=ORIENTED_EDGE('',*,*,#2955,.T.);
#3817=ORIENTED_EDGE('',*,*,#2956,.F.);
#3818=ORIENTED_EDGE('',*,*,#2955,.F.);
#3819=ORIENTED_EDGE('',*,*,#2957,.F.);
#3820=ORIENTED_EDGE('',*,*,#2958,.T.);
#3821=ORIENTED_EDGE('',*,*,#2959,.F.);
#3822=ORIENTED_EDGE('',*,*,#2960,.F.);
#3823=ORIENTED_EDGE('',*,*,#2961,.T.);
#3824=ORIENTED_EDGE('',*,*,#2962,.F.);
#3825=ORIENTED_EDGE('',*,*,#2963,.F.);
#3826=ORIENTED_EDGE('',*,*,#2961,.F.);
#3827=ORIENTED_EDGE('',*,*,#2964,.F.);
#3828=ORIENTED_EDGE('',*,*,#2965,.F.);
#3829=ORIENTED_EDGE('',*,*,#2958,.F.);
#3830=ORIENTED_EDGE('',*,*,#2966,.F.);
#3831=ORIENTED_EDGE('',*,*,#2964,.T.);
#3832=ORIENTED_EDGE('',*,*,#2960,.T.);
#3833=ORIENTED_EDGE('',*,*,#2967,.F.);
#3834=ORIENTED_EDGE('',*,*,#2968,.T.);
#3835=ORIENTED_EDGE('',*,*,#2969,.F.);
#3836=ORIENTED_EDGE('',*,*,#2970,.F.);
#3837=ORIENTED_EDGE('',*,*,#2971,.F.);
#3838=ORIENTED_EDGE('',*,*,#2972,.T.);
#3839=ORIENTED_EDGE('',*,*,#2973,.F.);
#3840=ORIENTED_EDGE('',*,*,#2968,.F.);
#3841=ORIENTED_EDGE('',*,*,#2974,.F.);
#3842=ORIENTED_EDGE('',*,*,#2975,.F.);
#3843=ORIENTED_EDGE('',*,*,#2976,.F.);
#3844=ORIENTED_EDGE('',*,*,#2972,.F.);
#3845=ORIENTED_EDGE('',*,*,#2977,.F.);
#3846=ORIENTED_EDGE('',*,*,#2974,.T.);
#3847=ORIENTED_EDGE('',*,*,#2971,.T.);
#3848=ORIENTED_EDGE('',*,*,#2967,.T.);
#3849=ORIENTED_EDGE('',*,*,#2978,.F.);
#3850=ORIENTED_EDGE('',*,*,#2979,.F.);
#3851=ORIENTED_EDGE('',*,*,#2980,.T.);
#3852=ORIENTED_EDGE('',*,*,#2981,.F.);
#3853=ORIENTED_EDGE('',*,*,#2980,.F.);
#3854=ORIENTED_EDGE('',*,*,#2979,.T.);
#3855=ORIENTED_EDGE('',*,*,#2976,.T.);
#3856=ORIENTED_EDGE('',*,*,#2982,.F.);
#3857=ORIENTED_EDGE('',*,*,#2969,.T.);
#3858=ORIENTED_EDGE('',*,*,#2973,.T.);
#3859=ORIENTED_EDGE('',*,*,#2983,.F.);
#3860=ORIENTED_EDGE('',*,*,#2984,.F.);
#3861=ORIENTED_EDGE('',*,*,#2954,.T.);
#3862=ORIENTED_EDGE('',*,*,#2951,.T.);
#3863=ORIENTED_EDGE('',*,*,#2948,.T.);
#3864=ORIENTED_EDGE('',*,*,#2945,.T.);
#3865=ORIENTED_EDGE('',*,*,#2985,.F.);
#3866=ORIENTED_EDGE('',*,*,#2986,.T.);
#3867=ORIENTED_EDGE('',*,*,#2983,.T.);
#3868=ORIENTED_EDGE('',*,*,#2986,.F.);
#3869=ORIENTED_EDGE('',*,*,#2975,.T.);
#3870=ORIENTED_EDGE('',*,*,#2978,.T.);
#3871=ORIENTED_EDGE('',*,*,#2970,.T.);
#3872=ORIENTED_EDGE('',*,*,#2982,.T.);
#3873=ORIENTED_EDGE('',*,*,#2965,.T.);
#3874=ORIENTED_EDGE('',*,*,#2966,.T.);
#3875=ORIENTED_EDGE('',*,*,#2959,.T.);
#3876=ORIENTED_EDGE('',*,*,#2957,.T.);
#3877=ORIENTED_EDGE('',*,*,#2984,.T.);
#3878=ORIENTED_EDGE('',*,*,#2987,.T.);
#3879=ORIENTED_EDGE('',*,*,#2977,.T.);
#3880=ORIENTED_EDGE('',*,*,#2987,.F.);
#3881=ORIENTED_EDGE('',*,*,#2962,.T.);
#3882=ORIENTED_EDGE('',*,*,#2963,.T.);
#3883=ORIENTED_EDGE('',*,*,#2985,.T.);
#3884=ORIENTED_EDGE('',*,*,#2981,.T.);
#3885=ORIENTED_EDGE('',*,*,#2956,.T.);
#3886=ORIENTED_EDGE('',*,*,#2953,.T.);
#3887=ORIENTED_EDGE('',*,*,#2950,.T.);
#3888=ORIENTED_EDGE('',*,*,#2947,.T.);
#3889=ORIENTED_EDGE('',*,*,#2988,.F.);
#3890=ORIENTED_EDGE('',*,*,#2989,.T.);
#3891=ORIENTED_EDGE('',*,*,#2990,.T.);
#3892=ORIENTED_EDGE('',*,*,#2989,.F.);
#3893=ORIENTED_EDGE('',*,*,#2991,.F.);
#3894=ORIENTED_EDGE('',*,*,#2992,.T.);
#3895=ORIENTED_EDGE('',*,*,#2993,.T.);
#3896=ORIENTED_EDGE('',*,*,#2992,.F.);
#3897=ORIENTED_EDGE('',*,*,#2991,.T.);
#3898=ORIENTED_EDGE('',*,*,#2988,.T.);
#3899=ORIENTED_EDGE('',*,*,#2993,.F.);
#3900=ORIENTED_EDGE('',*,*,#2990,.F.);
#3901=ORIENTED_EDGE('',*,*,#2994,.F.);
#3902=ORIENTED_EDGE('',*,*,#2995,.T.);
#3903=ORIENTED_EDGE('',*,*,#2996,.F.);
#3904=ORIENTED_EDGE('',*,*,#2995,.F.);
#3905=ORIENTED_EDGE('',*,*,#2994,.T.);
#3906=ORIENTED_EDGE('',*,*,#2997,.F.);
#3907=ORIENTED_EDGE('',*,*,#2998,.T.);
#3908=ORIENTED_EDGE('',*,*,#2999,.F.);
#3909=ORIENTED_EDGE('',*,*,#3000,.T.);
#3910=ORIENTED_EDGE('',*,*,#3001,.F.);
#3911=ORIENTED_EDGE('',*,*,#3000,.F.);
#3912=ORIENTED_EDGE('',*,*,#3002,.F.);
#3913=ORIENTED_EDGE('',*,*,#3003,.F.);
#3914=ORIENTED_EDGE('',*,*,#3004,.F.);
#3915=ORIENTED_EDGE('',*,*,#3003,.T.);
#3916=ORIENTED_EDGE('',*,*,#3005,.T.);
#3917=ORIENTED_EDGE('',*,*,#3006,.T.);
#3918=ORIENTED_EDGE('',*,*,#3002,.T.);
#3919=ORIENTED_EDGE('',*,*,#2999,.T.);
#3920=ORIENTED_EDGE('',*,*,#3007,.T.);
#3921=ORIENTED_EDGE('',*,*,#3005,.F.);
#3922=ORIENTED_EDGE('',*,*,#3008,.F.);
#3923=ORIENTED_EDGE('',*,*,#3006,.F.);
#3924=ORIENTED_EDGE('',*,*,#3007,.F.);
#3925=ORIENTED_EDGE('',*,*,#2998,.F.);
#3926=ORIENTED_EDGE('',*,*,#3009,.F.);
#3927=ORIENTED_EDGE('',*,*,#3010,.T.);
#3928=ORIENTED_EDGE('',*,*,#3011,.T.);
#3929=ORIENTED_EDGE('',*,*,#3010,.F.);
#3930=ORIENTED_EDGE('',*,*,#3004,.T.);
#3931=ORIENTED_EDGE('',*,*,#3008,.T.);
#3932=ORIENTED_EDGE('',*,*,#2997,.T.);
#3933=ORIENTED_EDGE('',*,*,#3001,.T.);
#3934=ORIENTED_EDGE('',*,*,#3009,.T.);
#3935=ORIENTED_EDGE('',*,*,#2996,.T.);
#3936=ORIENTED_EDGE('',*,*,#3011,.F.);
#3937=ORIENTED_EDGE('',*,*,#3012,.F.);
#3938=ORIENTED_EDGE('',*,*,#3013,.T.);
#3939=ORIENTED_EDGE('',*,*,#3014,.F.);
#3940=ORIENTED_EDGE('',*,*,#3013,.F.);
#3941=ORIENTED_EDGE('',*,*,#3015,.F.);
#3942=ORIENTED_EDGE('',*,*,#3016,.T.);
#3943=ORIENTED_EDGE('',*,*,#3017,.F.);
#3944=ORIENTED_EDGE('',*,*,#3016,.F.);
#3945=ORIENTED_EDGE('',*,*,#3018,.F.);
#3946=ORIENTED_EDGE('',*,*,#3019,.T.);
#3947=ORIENTED_EDGE('',*,*,#3020,.F.);
#3948=ORIENTED_EDGE('',*,*,#3019,.F.);
#3949=ORIENTED_EDGE('',*,*,#3021,.F.);
#3950=ORIENTED_EDGE('',*,*,#3022,.T.);
#3951=ORIENTED_EDGE('',*,*,#3023,.F.);
#3952=ORIENTED_EDGE('',*,*,#3022,.F.);
#3953=ORIENTED_EDGE('',*,*,#3024,.F.);
#3954=ORIENTED_EDGE('',*,*,#3025,.T.);
#3955=ORIENTED_EDGE('',*,*,#3026,.F.);
#3956=ORIENTED_EDGE('',*,*,#3027,.F.);
#3957=ORIENTED_EDGE('',*,*,#3028,.T.);
#3958=ORIENTED_EDGE('',*,*,#3029,.F.);
#3959=ORIENTED_EDGE('',*,*,#3030,.F.);
#3960=ORIENTED_EDGE('',*,*,#3028,.F.);
#3961=ORIENTED_EDGE('',*,*,#3031,.F.);
#3962=ORIENTED_EDGE('',*,*,#3032,.F.);
#3963=ORIENTED_EDGE('',*,*,#3025,.F.);
#3964=ORIENTED_EDGE('',*,*,#3033,.F.);
#3965=ORIENTED_EDGE('',*,*,#3031,.T.);
#3966=ORIENTED_EDGE('',*,*,#3027,.T.);
#3967=ORIENTED_EDGE('',*,*,#3034,.F.);
#3968=ORIENTED_EDGE('',*,*,#3035,.F.);
#3969=ORIENTED_EDGE('',*,*,#3036,.F.);
#3970=ORIENTED_EDGE('',*,*,#3037,.F.);
#3971=ORIENTED_EDGE('',*,*,#3038,.F.);
#3972=ORIENTED_EDGE('',*,*,#3039,.F.);
#3973=ORIENTED_EDGE('',*,*,#3040,.F.);
#3974=ORIENTED_EDGE('',*,*,#3041,.T.);
#3975=ORIENTED_EDGE('',*,*,#3042,.F.);
#3976=ORIENTED_EDGE('',*,*,#3041,.F.);
#3977=ORIENTED_EDGE('',*,*,#3043,.F.);
#3978=ORIENTED_EDGE('',*,*,#3035,.T.);
#3979=ORIENTED_EDGE('',*,*,#3044,.F.);
#3980=ORIENTED_EDGE('',*,*,#3036,.T.);
#3981=ORIENTED_EDGE('',*,*,#3043,.T.);
#3982=ORIENTED_EDGE('',*,*,#3040,.T.);
#3983=ORIENTED_EDGE('',*,*,#3045,.F.);
#3984=ORIENTED_EDGE('',*,*,#3037,.T.);
#3985=ORIENTED_EDGE('',*,*,#3045,.T.);
#3986=ORIENTED_EDGE('',*,*,#3039,.T.);
#3987=ORIENTED_EDGE('',*,*,#3046,.F.);
#3988=ORIENTED_EDGE('',*,*,#3032,.T.);
#3989=ORIENTED_EDGE('',*,*,#3033,.T.);
#3990=ORIENTED_EDGE('',*,*,#3026,.T.);
#3991=ORIENTED_EDGE('',*,*,#3024,.T.);
#3992=ORIENTED_EDGE('',*,*,#3047,.F.);
#3993=ORIENTED_EDGE('',*,*,#3048,.T.);
#3994=ORIENTED_EDGE('',*,*,#3044,.T.);
#3995=ORIENTED_EDGE('',*,*,#3048,.F.);
#3996=ORIENTED_EDGE('',*,*,#3049,.T.);
#3997=ORIENTED_EDGE('',*,*,#3050,.F.);
#3998=ORIENTED_EDGE('',*,*,#3023,.T.);
#3999=ORIENTED_EDGE('',*,*,#3020,.T.);
#4000=ORIENTED_EDGE('',*,*,#3017,.T.);
#4001=ORIENTED_EDGE('',*,*,#3014,.T.);
#4002=ORIENTED_EDGE('',*,*,#3049,.F.);
#4003=ORIENTED_EDGE('',*,*,#3051,.T.);
#4004=ORIENTED_EDGE('',*,*,#3052,.T.);
#4005=ORIENTED_EDGE('',*,*,#3051,.F.);
#4006=ORIENTED_EDGE('',*,*,#3053,.F.);
#4007=ORIENTED_EDGE('',*,*,#3054,.T.);
#4008=ORIENTED_EDGE('',*,*,#3050,.T.);
#4009=ORIENTED_EDGE('',*,*,#3054,.F.);
#4010=ORIENTED_EDGE('',*,*,#3029,.T.);
#4011=ORIENTED_EDGE('',*,*,#3030,.T.);
#4012=ORIENTED_EDGE('',*,*,#3053,.T.);
#4013=ORIENTED_EDGE('',*,*,#3034,.T.);
#4014=ORIENTED_EDGE('',*,*,#3046,.T.);
#4015=ORIENTED_EDGE('',*,*,#3038,.T.);
#4016=ORIENTED_EDGE('',*,*,#3042,.T.);
#4017=ORIENTED_EDGE('',*,*,#3052,.F.);
#4018=ORIENTED_EDGE('',*,*,#3047,.T.);
#4019=ORIENTED_EDGE('',*,*,#3021,.T.);
#4020=ORIENTED_EDGE('',*,*,#3018,.T.);
#4021=ORIENTED_EDGE('',*,*,#3015,.T.);
#4022=ORIENTED_EDGE('',*,*,#3012,.T.);
#4023=ORIENTED_EDGE('',*,*,#3055,.F.);
#4024=ORIENTED_EDGE('',*,*,#3056,.T.);
#4025=ORIENTED_EDGE('',*,*,#3057,.T.);
#4026=ORIENTED_EDGE('',*,*,#3056,.F.);
#4027=ORIENTED_EDGE('',*,*,#3058,.F.);
#4028=ORIENTED_EDGE('',*,*,#3059,.T.);
#4029=ORIENTED_EDGE('',*,*,#3060,.T.);
#4030=ORIENTED_EDGE('',*,*,#3059,.F.);
#4031=ORIENTED_EDGE('',*,*,#3058,.T.);
#4032=ORIENTED_EDGE('',*,*,#3055,.T.);
#4033=ORIENTED_EDGE('',*,*,#3060,.F.);
#4034=ORIENTED_EDGE('',*,*,#3057,.F.);
#4035=ORIENTED_EDGE('',*,*,#3061,.F.);
#4036=ORIENTED_EDGE('',*,*,#3062,.T.);
#4037=ORIENTED_EDGE('',*,*,#3063,.T.);
#4038=ORIENTED_EDGE('',*,*,#3062,.F.);
#4039=ORIENTED_EDGE('',*,*,#3064,.F.);
#4040=ORIENTED_EDGE('',*,*,#3065,.T.);
#4041=ORIENTED_EDGE('',*,*,#3066,.T.);
#4042=ORIENTED_EDGE('',*,*,#3065,.F.);
#4043=ORIENTED_EDGE('',*,*,#3064,.T.);
#4044=ORIENTED_EDGE('',*,*,#3061,.T.);
#4045=ORIENTED_EDGE('',*,*,#3066,.F.);
#4046=ORIENTED_EDGE('',*,*,#3063,.F.);
#4047=ORIENTED_EDGE('',*,*,#3067,.F.);
#4048=ORIENTED_EDGE('',*,*,#3068,.T.);
#4049=ORIENTED_EDGE('',*,*,#3069,.F.);
#4050=ORIENTED_EDGE('',*,*,#3070,.F.);
#4051=ORIENTED_EDGE('',*,*,#3071,.T.);
#4052=ORIENTED_EDGE('',*,*,#3072,.F.);
#4053=ORIENTED_EDGE('',*,*,#3073,.F.);
#4054=ORIENTED_EDGE('',*,*,#3071,.F.);
#4055=ORIENTED_EDGE('',*,*,#3074,.F.);
#4056=ORIENTED_EDGE('',*,*,#3075,.F.);
#4057=ORIENTED_EDGE('',*,*,#3068,.F.);
#4058=ORIENTED_EDGE('',*,*,#3076,.F.);
#4059=ORIENTED_EDGE('',*,*,#3074,.T.);
#4060=ORIENTED_EDGE('',*,*,#3070,.T.);
#4061=ORIENTED_EDGE('',*,*,#3077,.F.);
#4062=ORIENTED_EDGE('',*,*,#3078,.T.);
#4063=ORIENTED_EDGE('',*,*,#3079,.T.);
#4064=ORIENTED_EDGE('',*,*,#3078,.F.);
#4065=ORIENTED_EDGE('',*,*,#3075,.T.);
#4066=ORIENTED_EDGE('',*,*,#3076,.T.);
#4067=ORIENTED_EDGE('',*,*,#3069,.T.);
#4068=ORIENTED_EDGE('',*,*,#3067,.T.);
#4069=ORIENTED_EDGE('',*,*,#3080,.F.);
#4070=ORIENTED_EDGE('',*,*,#3081,.T.);
#4071=ORIENTED_EDGE('',*,*,#3082,.T.);
#4072=ORIENTED_EDGE('',*,*,#3081,.F.);
#4073=ORIENTED_EDGE('',*,*,#3072,.T.);
#4074=ORIENTED_EDGE('',*,*,#3073,.T.);
#4075=ORIENTED_EDGE('',*,*,#3080,.T.);
#4076=ORIENTED_EDGE('',*,*,#3077,.T.);
#4077=ORIENTED_EDGE('',*,*,#3082,.F.);
#4078=ORIENTED_EDGE('',*,*,#3079,.F.);
#4079=ORIENTED_EDGE('',*,*,#3083,.F.);
#4080=ORIENTED_EDGE('',*,*,#3084,.T.);
#4081=ORIENTED_EDGE('',*,*,#3085,.F.);
#4082=ORIENTED_EDGE('',*,*,#3086,.F.);
#4083=ORIENTED_EDGE('',*,*,#3087,.T.);
#4084=ORIENTED_EDGE('',*,*,#3088,.F.);
#4085=ORIENTED_EDGE('',*,*,#3089,.F.);
#4086=ORIENTED_EDGE('',*,*,#3087,.F.);
#4087=ORIENTED_EDGE('',*,*,#3090,.F.);
#4088=ORIENTED_EDGE('',*,*,#3091,.F.);
#4089=ORIENTED_EDGE('',*,*,#3084,.F.);
#4090=ORIENTED_EDGE('',*,*,#3092,.F.);
#4091=ORIENTED_EDGE('',*,*,#3090,.T.);
#4092=ORIENTED_EDGE('',*,*,#3086,.T.);
#4093=ORIENTED_EDGE('',*,*,#3093,.F.);
#4094=ORIENTED_EDGE('',*,*,#3094,.T.);
#4095=ORIENTED_EDGE('',*,*,#3095,.T.);
#4096=ORIENTED_EDGE('',*,*,#3094,.F.);
#4097=ORIENTED_EDGE('',*,*,#3091,.T.);
#4098=ORIENTED_EDGE('',*,*,#3092,.T.);
#4099=ORIENTED_EDGE('',*,*,#3085,.T.);
#4100=ORIENTED_EDGE('',*,*,#3083,.T.);
#4101=ORIENTED_EDGE('',*,*,#3096,.F.);
#4102=ORIENTED_EDGE('',*,*,#3097,.T.);
#4103=ORIENTED_EDGE('',*,*,#3098,.T.);
#4104=ORIENTED_EDGE('',*,*,#3097,.F.);
#4105=ORIENTED_EDGE('',*,*,#3088,.T.);
#4106=ORIENTED_EDGE('',*,*,#3089,.T.);
#4107=ORIENTED_EDGE('',*,*,#3096,.T.);
#4108=ORIENTED_EDGE('',*,*,#3093,.T.);
#4109=ORIENTED_EDGE('',*,*,#3098,.F.);
#4110=ORIENTED_EDGE('',*,*,#3095,.F.);
#4111=ORIENTED_EDGE('',*,*,#3099,.F.);
#4112=ORIENTED_EDGE('',*,*,#3100,.F.);
#4113=ORIENTED_EDGE('',*,*,#3101,.F.);
#4114=ORIENTED_EDGE('',*,*,#3102,.F.);
#4115=ORIENTED_EDGE('',*,*,#3103,.F.);
#4116=ORIENTED_EDGE('',*,*,#3104,.F.);
#4117=ORIENTED_EDGE('',*,*,#3105,.F.);
#4118=ORIENTED_EDGE('',*,*,#3106,.F.);
#4119=ORIENTED_EDGE('',*,*,#3103,.T.);
#4120=ORIENTED_EDGE('',*,*,#3107,.T.);
#4121=ORIENTED_EDGE('',*,*,#3108,.T.);
#4122=ORIENTED_EDGE('',*,*,#3109,.T.);
#4123=ORIENTED_EDGE('',*,*,#3102,.T.);
#4124=ORIENTED_EDGE('',*,*,#3110,.F.);
#4125=ORIENTED_EDGE('',*,*,#3111,.T.);
#4126=ORIENTED_EDGE('',*,*,#3107,.F.);
#4127=ORIENTED_EDGE('',*,*,#3101,.T.);
#4128=ORIENTED_EDGE('',*,*,#3112,.T.);
#4129=ORIENTED_EDGE('',*,*,#3113,.T.);
#4130=ORIENTED_EDGE('',*,*,#3110,.T.);
#4131=ORIENTED_EDGE('',*,*,#3100,.T.);
#4132=ORIENTED_EDGE('',*,*,#3114,.F.);
#4133=ORIENTED_EDGE('',*,*,#3115,.T.);
#4134=ORIENTED_EDGE('',*,*,#3112,.F.);
#4135=ORIENTED_EDGE('',*,*,#3116,.F.);
#4136=ORIENTED_EDGE('',*,*,#3117,.F.);
#4137=ORIENTED_EDGE('',*,*,#3108,.F.);
#4138=ORIENTED_EDGE('',*,*,#3111,.F.);
#4139=ORIENTED_EDGE('',*,*,#3113,.F.);
#4140=ORIENTED_EDGE('',*,*,#3115,.F.);
#4141=ORIENTED_EDGE('',*,*,#3118,.F.);
#4142=ORIENTED_EDGE('',*,*,#3119,.F.);
#4143=ORIENTED_EDGE('',*,*,#3104,.T.);
#4144=ORIENTED_EDGE('',*,*,#3109,.F.);
#4145=ORIENTED_EDGE('',*,*,#3117,.T.);
#4146=ORIENTED_EDGE('',*,*,#3120,.F.);
#4147=ORIENTED_EDGE('',*,*,#3099,.T.);
#4148=ORIENTED_EDGE('',*,*,#3121,.T.);
#4149=ORIENTED_EDGE('',*,*,#3118,.T.);
#4150=ORIENTED_EDGE('',*,*,#3114,.T.);
#4151=ORIENTED_EDGE('',*,*,#3105,.T.);
#4152=ORIENTED_EDGE('',*,*,#3120,.T.);
#4153=ORIENTED_EDGE('',*,*,#3116,.T.);
#4154=ORIENTED_EDGE('',*,*,#3122,.T.);
#4155=ORIENTED_EDGE('',*,*,#3106,.T.);
#4156=ORIENTED_EDGE('',*,*,#3122,.F.);
#4157=ORIENTED_EDGE('',*,*,#3119,.T.);
#4158=ORIENTED_EDGE('',*,*,#3121,.F.);
#4159=ORIENTED_EDGE('',*,*,#3123,.F.);
#4160=ORIENTED_EDGE('',*,*,#3124,.F.);
#4161=ORIENTED_EDGE('',*,*,#3125,.T.);
#4162=ORIENTED_EDGE('',*,*,#3123,.T.);
#4163=ORIENTED_EDGE('',*,*,#3125,.F.);
#4164=ORIENTED_EDGE('',*,*,#3126,.F.);
#4165=ORIENTED_EDGE('',*,*,#3127,.T.);
#4166=ORIENTED_EDGE('',*,*,#3124,.T.);
#4167=ORIENTED_EDGE('',*,*,#3127,.F.);
#4168=ORIENTED_EDGE('',*,*,#3128,.F.);
#4169=ORIENTED_EDGE('',*,*,#3129,.T.);
#4170=ORIENTED_EDGE('',*,*,#3126,.T.);
#4171=ORIENTED_EDGE('',*,*,#3129,.F.);
#4172=ORIENTED_EDGE('',*,*,#3128,.T.);
#4173=ORIENTED_EDGE('',*,*,#3130,.F.);
#4174=ORIENTED_EDGE('',*,*,#3131,.F.);
#4175=ORIENTED_EDGE('',*,*,#3132,.T.);
#4176=ORIENTED_EDGE('',*,*,#3130,.T.);
#4177=ORIENTED_EDGE('',*,*,#3132,.F.);
#4178=ORIENTED_EDGE('',*,*,#3133,.F.);
#4179=ORIENTED_EDGE('',*,*,#3134,.T.);
#4180=ORIENTED_EDGE('',*,*,#3131,.T.);
#4181=ORIENTED_EDGE('',*,*,#3134,.F.);
#4182=ORIENTED_EDGE('',*,*,#3135,.F.);
#4183=ORIENTED_EDGE('',*,*,#3136,.T.);
#4184=ORIENTED_EDGE('',*,*,#3133,.T.);
#4185=ORIENTED_EDGE('',*,*,#3136,.F.);
#4186=ORIENTED_EDGE('',*,*,#3135,.T.);
#4187=ORIENTED_EDGE('',*,*,#3137,.T.);
#4188=ORIENTED_EDGE('',*,*,#3138,.T.);
#4189=ORIENTED_EDGE('',*,*,#3139,.T.);
#4190=ORIENTED_EDGE('',*,*,#3140,.F.);
#4191=ORIENTED_EDGE('',*,*,#3141,.T.);
#4192=ORIENTED_EDGE('',*,*,#3142,.T.);
#4193=ORIENTED_EDGE('',*,*,#3143,.T.);
#4194=ORIENTED_EDGE('',*,*,#3138,.F.);
#4195=ORIENTED_EDGE('',*,*,#3144,.T.);
#4196=ORIENTED_EDGE('',*,*,#3145,.T.);
#4197=ORIENTED_EDGE('',*,*,#3146,.T.);
#4198=ORIENTED_EDGE('',*,*,#3142,.F.);
#4199=ORIENTED_EDGE('',*,*,#3147,.T.);
#4200=ORIENTED_EDGE('',*,*,#3148,.T.);
#4201=ORIENTED_EDGE('',*,*,#3149,.T.);
#4202=ORIENTED_EDGE('',*,*,#3145,.F.);
#4203=ORIENTED_EDGE('',*,*,#3150,.T.);
#4204=ORIENTED_EDGE('',*,*,#3151,.T.);
#4205=ORIENTED_EDGE('',*,*,#3152,.T.);
#4206=ORIENTED_EDGE('',*,*,#3148,.F.);
#4207=ORIENTED_EDGE('',*,*,#3153,.T.);
#4208=ORIENTED_EDGE('',*,*,#3140,.T.);
#4209=ORIENTED_EDGE('',*,*,#3154,.T.);
#4210=ORIENTED_EDGE('',*,*,#3151,.F.);
#4211=ORIENTED_EDGE('',*,*,#3153,.F.);
#4212=ORIENTED_EDGE('',*,*,#3150,.F.);
#4213=ORIENTED_EDGE('',*,*,#3147,.F.);
#4214=ORIENTED_EDGE('',*,*,#3144,.F.);
#4215=ORIENTED_EDGE('',*,*,#3141,.F.);
#4216=ORIENTED_EDGE('',*,*,#3137,.F.);
#4217=ORIENTED_EDGE('',*,*,#3154,.F.);
#4218=ORIENTED_EDGE('',*,*,#3139,.F.);
#4219=ORIENTED_EDGE('',*,*,#3143,.F.);
#4220=ORIENTED_EDGE('',*,*,#3146,.F.);
#4221=ORIENTED_EDGE('',*,*,#3149,.F.);
#4222=ORIENTED_EDGE('',*,*,#3152,.F.);
#4223=ORIENTED_EDGE('',*,*,#3155,.F.);
#4224=ORIENTED_EDGE('',*,*,#3156,.F.);
#4225=ORIENTED_EDGE('',*,*,#3157,.T.);
#4226=ORIENTED_EDGE('',*,*,#3155,.T.);
#4227=ORIENTED_EDGE('',*,*,#3157,.F.);
#4228=ORIENTED_EDGE('',*,*,#3158,.F.);
#4229=ORIENTED_EDGE('',*,*,#3159,.T.);
#4230=ORIENTED_EDGE('',*,*,#3156,.T.);
#4231=ORIENTED_EDGE('',*,*,#3159,.F.);
#4232=ORIENTED_EDGE('',*,*,#3160,.F.);
#4233=ORIENTED_EDGE('',*,*,#3161,.T.);
#4234=ORIENTED_EDGE('',*,*,#3158,.T.);
#4235=ORIENTED_EDGE('',*,*,#3161,.F.);
#4236=ORIENTED_EDGE('',*,*,#3160,.T.);
#4237=ORIENTED_EDGE('',*,*,#3162,.F.);
#4238=ORIENTED_EDGE('',*,*,#3163,.F.);
#4239=ORIENTED_EDGE('',*,*,#3164,.T.);
#4240=ORIENTED_EDGE('',*,*,#3162,.T.);
#4241=ORIENTED_EDGE('',*,*,#3164,.F.);
#4242=ORIENTED_EDGE('',*,*,#3165,.F.);
#4243=ORIENTED_EDGE('',*,*,#3166,.T.);
#4244=ORIENTED_EDGE('',*,*,#3163,.T.);
#4245=ORIENTED_EDGE('',*,*,#3166,.F.);
#4246=ORIENTED_EDGE('',*,*,#3167,.F.);
#4247=ORIENTED_EDGE('',*,*,#3168,.T.);
#4248=ORIENTED_EDGE('',*,*,#3165,.T.);
#4249=ORIENTED_EDGE('',*,*,#3168,.F.);
#4250=ORIENTED_EDGE('',*,*,#3167,.T.);
#4251=ORIENTED_EDGE('',*,*,#3169,.T.);
#4252=ORIENTED_EDGE('',*,*,#3170,.T.);
#4253=ORIENTED_EDGE('',*,*,#3171,.T.);
#4254=ORIENTED_EDGE('',*,*,#3172,.F.);
#4255=ORIENTED_EDGE('',*,*,#3173,.T.);
#4256=ORIENTED_EDGE('',*,*,#3174,.T.);
#4257=ORIENTED_EDGE('',*,*,#3175,.T.);
#4258=ORIENTED_EDGE('',*,*,#3170,.F.);
#4259=ORIENTED_EDGE('',*,*,#3176,.T.);
#4260=ORIENTED_EDGE('',*,*,#3177,.T.);
#4261=ORIENTED_EDGE('',*,*,#3178,.T.);
#4262=ORIENTED_EDGE('',*,*,#3174,.F.);
#4263=ORIENTED_EDGE('',*,*,#3179,.T.);
#4264=ORIENTED_EDGE('',*,*,#3180,.T.);
#4265=ORIENTED_EDGE('',*,*,#3181,.T.);
#4266=ORIENTED_EDGE('',*,*,#3177,.F.);
#4267=ORIENTED_EDGE('',*,*,#3182,.T.);
#4268=ORIENTED_EDGE('',*,*,#3183,.T.);
#4269=ORIENTED_EDGE('',*,*,#3184,.T.);
#4270=ORIENTED_EDGE('',*,*,#3180,.F.);
#4271=ORIENTED_EDGE('',*,*,#3185,.T.);
#4272=ORIENTED_EDGE('',*,*,#3172,.T.);
#4273=ORIENTED_EDGE('',*,*,#3186,.T.);
#4274=ORIENTED_EDGE('',*,*,#3183,.F.);
#4275=ORIENTED_EDGE('',*,*,#3185,.F.);
#4276=ORIENTED_EDGE('',*,*,#3182,.F.);
#4277=ORIENTED_EDGE('',*,*,#3179,.F.);
#4278=ORIENTED_EDGE('',*,*,#3176,.F.);
#4279=ORIENTED_EDGE('',*,*,#3173,.F.);
#4280=ORIENTED_EDGE('',*,*,#3169,.F.);
#4281=ORIENTED_EDGE('',*,*,#3186,.F.);
#4282=ORIENTED_EDGE('',*,*,#3171,.F.);
#4283=ORIENTED_EDGE('',*,*,#3175,.F.);
#4284=ORIENTED_EDGE('',*,*,#3178,.F.);
#4285=ORIENTED_EDGE('',*,*,#3181,.F.);
#4286=ORIENTED_EDGE('',*,*,#3184,.F.);
#4287=ORIENTED_EDGE('',*,*,#3187,.F.);
#4288=ORIENTED_EDGE('',*,*,#3188,.T.);
#4289=ORIENTED_EDGE('',*,*,#3189,.T.);
#4290=ORIENTED_EDGE('',*,*,#3188,.F.);
#4291=ORIENTED_EDGE('',*,*,#3190,.F.);
#4292=ORIENTED_EDGE('',*,*,#3191,.T.);
#4293=ORIENTED_EDGE('',*,*,#3192,.T.);
#4294=ORIENTED_EDGE('',*,*,#3191,.F.);
#4295=ORIENTED_EDGE('',*,*,#3190,.T.);
#4296=ORIENTED_EDGE('',*,*,#3187,.T.);
#4297=ORIENTED_EDGE('',*,*,#3192,.F.);
#4298=ORIENTED_EDGE('',*,*,#3189,.F.);
#4299=ORIENTED_EDGE('',*,*,#3193,.F.);
#4300=ORIENTED_EDGE('',*,*,#3194,.F.);
#4301=ORIENTED_EDGE('',*,*,#3195,.T.);
#4302=ORIENTED_EDGE('',*,*,#3196,.F.);
#4303=ORIENTED_EDGE('',*,*,#3195,.F.);
#4304=ORIENTED_EDGE('',*,*,#3197,.F.);
#4305=ORIENTED_EDGE('',*,*,#3198,.F.);
#4306=ORIENTED_EDGE('',*,*,#3199,.F.);
#4307=ORIENTED_EDGE('',*,*,#3200,.F.);
#4308=ORIENTED_EDGE('',*,*,#3201,.F.);
#4309=ORIENTED_EDGE('',*,*,#3202,.T.);
#4310=ORIENTED_EDGE('',*,*,#3203,.F.);
#4311=ORIENTED_EDGE('',*,*,#3204,.F.);
#4312=ORIENTED_EDGE('',*,*,#3205,.F.);
#4313=ORIENTED_EDGE('',*,*,#3206,.F.);
#4314=ORIENTED_EDGE('',*,*,#3207,.F.);
#4315=ORIENTED_EDGE('',*,*,#3208,.F.);
#4316=ORIENTED_EDGE('',*,*,#3202,.F.);
#4317=ORIENTED_EDGE('',*,*,#3198,.T.);
#4318=ORIENTED_EDGE('',*,*,#3209,.T.);
#4319=ORIENTED_EDGE('',*,*,#3207,.T.);
#4320=ORIENTED_EDGE('',*,*,#3210,.F.);
#4321=ORIENTED_EDGE('',*,*,#3197,.T.);
#4322=ORIENTED_EDGE('',*,*,#3211,.T.);
#4323=ORIENTED_EDGE('',*,*,#3208,.T.);
#4324=ORIENTED_EDGE('',*,*,#3209,.F.);
#4325=ORIENTED_EDGE('',*,*,#3194,.T.);
#4326=ORIENTED_EDGE('',*,*,#3212,.T.);
#4327=ORIENTED_EDGE('',*,*,#3203,.T.);
#4328=ORIENTED_EDGE('',*,*,#3211,.F.);
#4329=ORIENTED_EDGE('',*,*,#3213,.F.);
#4330=ORIENTED_EDGE('',*,*,#3214,.T.);
#4331=ORIENTED_EDGE('',*,*,#3215,.T.);
#4332=ORIENTED_EDGE('',*,*,#3214,.F.);
#4333=ORIENTED_EDGE('',*,*,#3193,.T.);
#4334=ORIENTED_EDGE('',*,*,#3216,.T.);
#4335=ORIENTED_EDGE('',*,*,#3204,.T.);
#4336=ORIENTED_EDGE('',*,*,#3212,.F.);
#4337=ORIENTED_EDGE('',*,*,#3199,.T.);
#4338=ORIENTED_EDGE('',*,*,#3210,.T.);
#4339=ORIENTED_EDGE('',*,*,#3206,.T.);
#4340=ORIENTED_EDGE('',*,*,#3217,.F.);
#4341=ORIENTED_EDGE('',*,*,#3200,.T.);
#4342=ORIENTED_EDGE('',*,*,#3217,.T.);
#4343=ORIENTED_EDGE('',*,*,#3205,.T.);
#4344=ORIENTED_EDGE('',*,*,#3216,.F.);
#4345=ORIENTED_EDGE('',*,*,#3201,.T.);
#4346=ORIENTED_EDGE('',*,*,#3213,.T.);
#4347=ORIENTED_EDGE('',*,*,#3196,.T.);
#4348=ORIENTED_EDGE('',*,*,#3215,.F.);
#4349=ORIENTED_EDGE('',*,*,#3218,.F.);
#4350=ORIENTED_EDGE('',*,*,#3219,.T.);
#4351=ORIENTED_EDGE('',*,*,#3220,.T.);
#4352=ORIENTED_EDGE('',*,*,#3221,.F.);
#4353=ORIENTED_EDGE('',*,*,#3222,.F.);
#4354=ORIENTED_EDGE('',*,*,#3223,.T.);
#4355=ORIENTED_EDGE('',*,*,#3224,.T.);
#4356=ORIENTED_EDGE('',*,*,#3219,.F.);
#4357=ORIENTED_EDGE('',*,*,#3225,.F.);
#4358=ORIENTED_EDGE('',*,*,#3226,.T.);
#4359=ORIENTED_EDGE('',*,*,#3227,.T.);
#4360=ORIENTED_EDGE('',*,*,#3223,.F.);
#4361=ORIENTED_EDGE('',*,*,#3228,.F.);
#4362=ORIENTED_EDGE('',*,*,#3229,.T.);
#4363=ORIENTED_EDGE('',*,*,#3230,.T.);
#4364=ORIENTED_EDGE('',*,*,#3226,.F.);
#4365=ORIENTED_EDGE('',*,*,#3231,.F.);
#4366=ORIENTED_EDGE('',*,*,#3232,.T.);
#4367=ORIENTED_EDGE('',*,*,#3233,.T.);
#4368=ORIENTED_EDGE('',*,*,#3229,.F.);
#4369=ORIENTED_EDGE('',*,*,#3234,.F.);
#4370=ORIENTED_EDGE('',*,*,#3221,.T.);
#4371=ORIENTED_EDGE('',*,*,#3235,.T.);
#4372=ORIENTED_EDGE('',*,*,#3232,.F.);
#4373=ORIENTED_EDGE('',*,*,#3235,.F.);
#4374=ORIENTED_EDGE('',*,*,#3220,.F.);
#4375=ORIENTED_EDGE('',*,*,#3224,.F.);
#4376=ORIENTED_EDGE('',*,*,#3227,.F.);
#4377=ORIENTED_EDGE('',*,*,#3230,.F.);
#4378=ORIENTED_EDGE('',*,*,#3233,.F.);
#4379=ORIENTED_EDGE('',*,*,#3236,.F.);
#4380=ORIENTED_EDGE('',*,*,#3218,.T.);
#4381=ORIENTED_EDGE('',*,*,#3234,.T.);
#4382=ORIENTED_EDGE('',*,*,#3231,.T.);
#4383=ORIENTED_EDGE('',*,*,#3228,.T.);
#4384=ORIENTED_EDGE('',*,*,#3225,.T.);
#4385=ORIENTED_EDGE('',*,*,#3222,.T.);
#4386=ORIENTED_EDGE('',*,*,#3237,.F.);
#4387=ORIENTED_EDGE('',*,*,#3238,.T.);
#4388=ORIENTED_EDGE('',*,*,#3236,.T.);
#4389=ORIENTED_EDGE('',*,*,#3238,.F.);
#4390=ORIENTED_EDGE('',*,*,#3239,.F.);
#4391=ORIENTED_EDGE('',*,*,#3240,.T.);
#4392=ORIENTED_EDGE('',*,*,#3237,.T.);
#4393=ORIENTED_EDGE('',*,*,#3240,.F.);
#4394=ORIENTED_EDGE('',*,*,#3241,.F.);
#4395=ORIENTED_EDGE('',*,*,#3242,.T.);
#4396=ORIENTED_EDGE('',*,*,#3239,.T.);
#4397=ORIENTED_EDGE('',*,*,#3242,.F.);
#4398=ORIENTED_EDGE('',*,*,#3241,.T.);
#4399=CYLINDRICAL_SURFACE('',#5096,0.25);
#4400=CYLINDRICAL_SURFACE('',#5099,0.25);
#4401=CYLINDRICAL_SURFACE('',#5102,0.25);
#4402=CYLINDRICAL_SURFACE('',#5105,0.25);
#4403=CYLINDRICAL_SURFACE('',#5129,0.34);
#4404=CYLINDRICAL_SURFACE('',#5132,0.34);
#4405=CYLINDRICAL_SURFACE('',#5135,0.33);
#4406=CYLINDRICAL_SURFACE('',#5138,0.33);
#4407=CYLINDRICAL_SURFACE('',#5148,0.425);
#4408=CYLINDRICAL_SURFACE('',#5151,0.645);
#4409=CYLINDRICAL_SURFACE('',#5157,0.425);
#4410=CYLINDRICAL_SURFACE('',#5160,0.645);
#4411=CYLINDRICAL_SURFACE('',#5166,0.34);
#4412=CYLINDRICAL_SURFACE('',#5169,0.34);
#4413=CYLINDRICAL_SURFACE('',#5172,0.33);
#4414=CYLINDRICAL_SURFACE('',#5175,0.33);
#4415=CYLINDRICAL_SURFACE('',#5185,0.425);
#4416=CYLINDRICAL_SURFACE('',#5188,0.645);
#4417=CYLINDRICAL_SURFACE('',#5194,0.425);
#4418=CYLINDRICAL_SURFACE('',#5197,0.645);
#4419=CYLINDRICAL_SURFACE('',#5204,2.05);
#4420=CYLINDRICAL_SURFACE('',#5207,2.05);
#4421=CYLINDRICAL_SURFACE('',#5225,2.8);
#4422=CYLINDRICAL_SURFACE('',#5235,0.65);
#4423=CYLINDRICAL_SURFACE('',#5237,0.65);
#4424=CYLINDRICAL_SURFACE('',#5245,1.8);
#4425=CYLINDRICAL_SURFACE('',#5254,0.25);
#4426=CYLINDRICAL_SURFACE('',#5255,0.25);
#4427=CYLINDRICAL_SURFACE('',#5256,1.65);
#4428=CYLINDRICAL_SURFACE('',#5259,0.25);
#4429=CYLINDRICAL_SURFACE('',#5260,0.25);
#4430=CYLINDRICAL_SURFACE('',#5261,0.25);
#4431=CYLINDRICAL_SURFACE('',#5262,0.25);
#4432=CYLINDRICAL_SURFACE('',#5267,1.75);
#4433=CYLINDRICAL_SURFACE('',#5271,1.);
#4434=CYLINDRICAL_SURFACE('',#5275,0.42);
#4435=CYLINDRICAL_SURFACE('',#5278,0.8);
#4436=CYLINDRICAL_SURFACE('',#5298,0.65);
#4437=CYLINDRICAL_SURFACE('',#5306,0.3933);
#4438=CYLINDRICAL_SURFACE('',#5309,0.21);
#4439=CYLINDRICAL_SURFACE('',#5320,1.);
#4440=CYLINDRICAL_SURFACE('',#5326,0.33);
#4441=CYLINDRICAL_SURFACE('',#5329,0.33);
#4442=CYLINDRICAL_SURFACE('',#5332,0.33);
#4443=CYLINDRICAL_SURFACE('',#5335,0.33);
#4444=CYLINDRICAL_SURFACE('',#5340,0.21);
#4445=CYLINDRICAL_SURFACE('',#5350,2.);
#4446=CYLINDRICAL_SURFACE('',#5358,4.);
#4447=CYLINDRICAL_SURFACE('',#5360,1.);
#4448=CYLINDRICAL_SURFACE('',#5361,1.7);
#4449=CYLINDRICAL_SURFACE('',#5364,0.275);
#4450=CYLINDRICAL_SURFACE('',#5367,1.1);
#4451=CYLINDRICAL_SURFACE('',#5373,0.21);
#4452=CYLINDRICAL_SURFACE('',#5384,1.);
#4453=CYLINDRICAL_SURFACE('',#5390,0.33);
#4454=CYLINDRICAL_SURFACE('',#5393,0.33);
#4455=CYLINDRICAL_SURFACE('',#5396,0.33);
#4456=CYLINDRICAL_SURFACE('',#5399,0.33);
#4457=CYLINDRICAL_SURFACE('',#5404,0.21);
#4458=CYLINDRICAL_SURFACE('',#5414,1.);
#4459=CYLINDRICAL_SURFACE('',#5416,2.);
#4460=CYLINDRICAL_SURFACE('',#5421,4.);
#4461=CYLINDRICAL_SURFACE('',#5423,1.7);
#4462=CYLINDRICAL_SURFACE('',#5428,0.275);
#4463=CYLINDRICAL_SURFACE('',#5431,1.1);
#4464=CYLINDRICAL_SURFACE('',#5437,1.);
#4465=CYLINDRICAL_SURFACE('',#5440,2.);
#4466=CYLINDRICAL_SURFACE('',#5448,0.21);
#4467=CYLINDRICAL_SURFACE('',#5452,1.005);
#4468=CYLINDRICAL_SURFACE('',#5455,1.5);
#4469=CYLINDRICAL_SURFACE('',#5463,0.21);
#4470=CYLINDRICAL_SURFACE('',#5467,1.005);
#4471=CYLINDRICAL_SURFACE('',#5470,1.5);
#4472=CYLINDRICAL_SURFACE('',#5491,0.425);
#4473=CYLINDRICAL_SURFACE('',#5499,0.24505);
#4474=CYLINDRICAL_SURFACE('',#5517,0.5);
#4475=CYLINDRICAL_SURFACE('',#5525,0.2942);
#4476=CYLINDRICAL_SURFACE('',#5539,0.32);
#4477=CYLINDRICAL_SURFACE('',#5542,0.6);
#4478=CYLINDRICAL_SURFACE('',#5582,0.25175);
#4479=CYLINDRICAL_SURFACE('',#5602,0.24505);
#4480=ADVANCED_FACE('',(#744),#4399,.F.);
#4481=ADVANCED_FACE('',(#745),#4400,.F.);
#4482=ADVANCED_FACE('',(#746),#4401,.F.);
#4483=ADVANCED_FACE('',(#747),#4402,.F.);
#4484=ADVANCED_FACE('',(#748),#570,.T.);
#4485=ADVANCED_FACE('',(#749),#571,.T.);
#4486=ADVANCED_FACE('',(#750),#572,.T.);
#4487=ADVANCED_FACE('',(#751),#573,.T.);
#4488=ADVANCED_FACE('',(#752,#453,#454,#455,#456),#574,.T.);
#4489=ADVANCED_FACE('',(#753,#457,#458,#459,#460),#575,.F.);
#4490=ADVANCED_FACE('',(#754),#576,.T.);
#4491=ADVANCED_FACE('',(#755),#577,.T.);
#4492=ADVANCED_FACE('',(#756),#578,.T.);
#4493=ADVANCED_FACE('',(#757),#579,.T.);
#4494=ADVANCED_FACE('',(#758),#580,.T.);
#4495=ADVANCED_FACE('',(#759),#581,.F.);
#4496=ADVANCED_FACE('',(#760),#582,.T.);
#4497=ADVANCED_FACE('',(#761),#583,.T.);
#4498=ADVANCED_FACE('',(#762),#584,.T.);
#4499=ADVANCED_FACE('',(#763),#585,.T.);
#4500=ADVANCED_FACE('',(#764),#586,.T.);
#4501=ADVANCED_FACE('',(#765),#587,.F.);
#4502=ADVANCED_FACE('',(#766),#4403,.F.);
#4503=ADVANCED_FACE('',(#767),#4404,.F.);
#4504=ADVANCED_FACE('',(#768),#4405,.F.);
#4505=ADVANCED_FACE('',(#769),#4406,.F.);
#4506=ADVANCED_FACE('',(#770),#588,.T.);
#4507=ADVANCED_FACE('',(#771),#589,.T.);
#4508=ADVANCED_FACE('',(#772),#590,.T.);
#4509=ADVANCED_FACE('',(#773),#591,.T.);
#4510=ADVANCED_FACE('',(#774,#461,#462,#463,#464),#592,.T.);
#4511=ADVANCED_FACE('',(#775,#465,#466,#467,#468),#593,.F.);
#4512=ADVANCED_FACE('',(#776),#4407,.F.);
#4513=ADVANCED_FACE('',(#777),#4408,.T.);
#4514=ADVANCED_FACE('',(#778,#469),#594,.T.);
#4515=ADVANCED_FACE('',(#779,#470),#595,.F.);
#4516=ADVANCED_FACE('',(#780),#4409,.F.);
#4517=ADVANCED_FACE('',(#781),#4410,.T.);
#4518=ADVANCED_FACE('',(#782,#471),#596,.T.);
#4519=ADVANCED_FACE('',(#783,#472),#597,.F.);
#4520=ADVANCED_FACE('',(#784),#4411,.F.);
#4521=ADVANCED_FACE('',(#785),#4412,.F.);
#4522=ADVANCED_FACE('',(#786),#4413,.F.);
#4523=ADVANCED_FACE('',(#787),#4414,.F.);
#4524=ADVANCED_FACE('',(#788),#598,.T.);
#4525=ADVANCED_FACE('',(#789),#599,.T.);
#4526=ADVANCED_FACE('',(#790),#600,.T.);
#4527=ADVANCED_FACE('',(#791),#601,.T.);
#4528=ADVANCED_FACE('',(#792,#473,#474,#475,#476),#602,.T.);
#4529=ADVANCED_FACE('',(#793,#477,#478,#479,#480),#603,.F.);
#4530=ADVANCED_FACE('',(#794),#4415,.F.);
#4531=ADVANCED_FACE('',(#795),#4416,.T.);
#4532=ADVANCED_FACE('',(#796,#481),#604,.T.);
#4533=ADVANCED_FACE('',(#797,#482),#605,.F.);
#4534=ADVANCED_FACE('',(#798),#4417,.F.);
#4535=ADVANCED_FACE('',(#799),#4418,.T.);
#4536=ADVANCED_FACE('',(#800,#483),#606,.T.);
#4537=ADVANCED_FACE('',(#801,#484),#607,.F.);
#4538=ADVANCED_FACE('',(#802),#4419,.F.);
#4539=ADVANCED_FACE('',(#803),#4420,.F.);
#4540=ADVANCED_FACE('',(#804,#485,#486),#340,.F.);
#4541=ADVANCED_FACE('',(#805),#608,.T.);
#4542=ADVANCED_FACE('',(#806),#609,.T.);
#4543=ADVANCED_FACE('',(#807),#610,.T.);
#4544=ADVANCED_FACE('',(#808),#611,.T.);
#4545=ADVANCED_FACE('',(#809),#612,.T.);
#4546=ADVANCED_FACE('',(#810),#613,.T.);
#4547=ADVANCED_FACE('',(#811,#487,#488,#489),#614,.T.);
#4548=ADVANCED_FACE('',(#812),#4421,.T.);
#4549=ADVANCED_FACE('',(#813,#490),#615,.F.);
#4550=ADVANCED_FACE('',(#814,#491),#616,.T.);
#4551=ADVANCED_FACE('',(#815),#617,.F.);
#4552=ADVANCED_FACE('',(#816),#618,.F.);
#4553=ADVANCED_FACE('',(#817),#619,.F.);
#4554=ADVANCED_FACE('',(#818),#620,.F.);
#4555=ADVANCED_FACE('',(#819),#621,.F.);
#4556=ADVANCED_FACE('',(#820),#4422,.F.);
#4557=ADVANCED_FACE('',(#821),#4423,.F.);
#4558=ADVANCED_FACE('',(#822),#622,.T.);
#4559=ADVANCED_FACE('',(#823),#623,.T.);
#4560=ADVANCED_FACE('',(#824),#624,.T.);
#4561=ADVANCED_FACE('',(#825),#625,.T.);
#4562=ADVANCED_FACE('',(#826,#492,#493,#494),#626,.F.);
#4563=ADVANCED_FACE('',(#827),#4424,.F.);
#4564=ADVANCED_FACE('',(#828,#495),#627,.T.);
#4565=ADVANCED_FACE('',(#829,#496,#497),#341,.T.);
#4566=ADVANCED_FACE('',(#830,#498),#628,.T.);
#4567=ADVANCED_FACE('',(#831),#4425,.F.);
#4568=ADVANCED_FACE('',(#832),#4426,.F.);
#4569=ADVANCED_FACE('',(#833,#499,#500,#501,#502,#503,#504),#4427,.T.);
#4570=ADVANCED_FACE('',(#834),#4428,.F.);
#4571=ADVANCED_FACE('',(#835),#4429,.F.);
#4572=ADVANCED_FACE('',(#836),#4430,.F.);
#4573=ADVANCED_FACE('',(#837),#4431,.F.);
#4574=ADVANCED_FACE('',(#838,#505),#629,.T.);
#4575=ADVANCED_FACE('',(#839,#506),#630,.T.);
#4576=ADVANCED_FACE('',(#840),#4432,.T.);
#4577=ADVANCED_FACE('',(#841,#507),#631,.T.);
#4578=ADVANCED_FACE('',(#842,#508,#509,#510,#511,#512,#513),#4433,.F.);
#4579=ADVANCED_FACE('',(#843),#4434,.F.);
#4580=ADVANCED_FACE('',(#844),#4435,.T.);
#4581=ADVANCED_FACE('',(#845,#514),#632,.T.);
#4582=ADVANCED_FACE('',(#846,#515),#633,.F.);
#4583=ADVANCED_FACE('',(#847),#634,.F.);
#4584=ADVANCED_FACE('',(#848),#635,.F.);
#4585=ADVANCED_FACE('',(#849),#636,.F.);
#4586=ADVANCED_FACE('',(#850),#637,.F.);
#4587=ADVANCED_FACE('',(#851),#638,.F.);
#4588=ADVANCED_FACE('',(#852),#639,.F.);
#4589=ADVANCED_FACE('',(#853),#640,.F.);
#4590=ADVANCED_FACE('',(#854),#641,.F.);
#4591=ADVANCED_FACE('',(#855),#642,.F.);
#4592=ADVANCED_FACE('',(#856),#643,.T.);
#4593=ADVANCED_FACE('',(#857),#23,.T.);
#4594=ADVANCED_FACE('',(#858),#4436,.T.);
#4595=ADVANCED_FACE('',(#859),#24,.T.);
#4596=ADVANCED_FACE('',(#860,#516),#644,.T.);
#4597=ADVANCED_FACE('',(#861),#25,.T.);
#4598=ADVANCED_FACE('',(#862),#4437,.T.);
#4599=ADVANCED_FACE('',(#863),#4438,.F.);
#4600=ADVANCED_FACE('',(#864),#645,.F.);
#4601=ADVANCED_FACE('',(#865),#646,.F.);
#4602=ADVANCED_FACE('',(#866),#647,.T.);
#4603=ADVANCED_FACE('',(#867),#648,.F.);
#4604=ADVANCED_FACE('',(#868),#649,.F.);
#4605=ADVANCED_FACE('',(#869),#650,.F.);
#4606=ADVANCED_FACE('',(#870,#517),#4439,.T.);
#4607=ADVANCED_FACE('',(#871),#651,.T.);
#4608=ADVANCED_FACE('',(#872,#518),#652,.F.);
#4609=ADVANCED_FACE('',(#873),#4440,.F.);
#4610=ADVANCED_FACE('',(#874),#4441,.F.);
#4611=ADVANCED_FACE('',(#875),#4442,.F.);
#4612=ADVANCED_FACE('',(#876),#4443,.F.);
#4613=ADVANCED_FACE('',(#877),#653,.T.);
#4614=ADVANCED_FACE('',(#878),#4444,.F.);
#4615=ADVANCED_FACE('',(#879),#654,.T.);
#4616=ADVANCED_FACE('',(#880),#655,.F.);
#4617=ADVANCED_FACE('',(#881),#656,.F.);
#4618=ADVANCED_FACE('',(#882),#657,.F.);
#4619=ADVANCED_FACE('',(#883,#519),#658,.F.);
#4620=ADVANCED_FACE('',(#884),#4445,.F.);
#4621=ADVANCED_FACE('',(#885,#520),#659,.T.);
#4622=ADVANCED_FACE('',(#886,#521,#522,#523,#524,#525),#660,.F.);
#4623=ADVANCED_FACE('',(#887),#4446,.T.);
#4624=ADVANCED_FACE('',(#888,#526),#4447,.F.);
#4625=ADVANCED_FACE('',(#889,#527),#4448,.T.);
#4626=ADVANCED_FACE('',(#890,#528,#529,#530,#531,#532),#661,.T.);
#4627=ADVANCED_FACE('',(#891),#4449,.F.);
#4628=ADVANCED_FACE('',(#892),#4450,.T.);
#4629=ADVANCED_FACE('',(#893,#533),#662,.T.);
#4630=ADVANCED_FACE('',(#894,#534),#663,.F.);
#4631=ADVANCED_FACE('',(#895),#4451,.F.);
#4632=ADVANCED_FACE('',(#896),#664,.T.);
#4633=ADVANCED_FACE('',(#897),#665,.F.);
#4634=ADVANCED_FACE('',(#898),#666,.T.);
#4635=ADVANCED_FACE('',(#899),#667,.F.);
#4636=ADVANCED_FACE('',(#900),#668,.F.);
#4637=ADVANCED_FACE('',(#901),#669,.F.);
#4638=ADVANCED_FACE('',(#902,#535),#4452,.T.);
#4639=ADVANCED_FACE('',(#903,#536),#670,.T.);
#4640=ADVANCED_FACE('',(#904),#671,.F.);
#4641=ADVANCED_FACE('',(#905),#4453,.F.);
#4642=ADVANCED_FACE('',(#906),#4454,.F.);
#4643=ADVANCED_FACE('',(#907),#4455,.F.);
#4644=ADVANCED_FACE('',(#908),#4456,.F.);
#4645=ADVANCED_FACE('',(#909),#672,.T.);
#4646=ADVANCED_FACE('',(#910),#4457,.F.);
#4647=ADVANCED_FACE('',(#911),#673,.T.);
#4648=ADVANCED_FACE('',(#912),#674,.F.);
#4649=ADVANCED_FACE('',(#913),#675,.F.);
#4650=ADVANCED_FACE('',(#914),#676,.F.);
#4651=ADVANCED_FACE('',(#915,#537),#677,.F.);
#4652=ADVANCED_FACE('',(#916,#538),#4458,.F.);
#4653=ADVANCED_FACE('',(#917),#4459,.F.);
#4654=ADVANCED_FACE('',(#918,#539,#540,#541,#542,#543),#678,.T.);
#4655=ADVANCED_FACE('',(#919),#4460,.T.);
#4656=ADVANCED_FACE('',(#920,#544),#4461,.T.);
#4657=ADVANCED_FACE('',(#921,#545),#679,.T.);
#4658=ADVANCED_FACE('',(#922,#546,#547,#548,#549,#550),#680,.F.);
#4659=ADVANCED_FACE('',(#923),#4462,.F.);
#4660=ADVANCED_FACE('',(#924),#4463,.T.);
#4661=ADVANCED_FACE('',(#925,#551),#681,.T.);
#4662=ADVANCED_FACE('',(#926,#552),#682,.F.);
#4663=ADVANCED_FACE('',(#927),#4464,.F.);
#4664=ADVANCED_FACE('',(#928),#4465,.T.);
#4665=ADVANCED_FACE('',(#929,#553),#683,.T.);
#4666=ADVANCED_FACE('',(#930,#554),#684,.F.);
#4667=ADVANCED_FACE('',(#931),#685,.T.);
#4668=ADVANCED_FACE('',(#932),#4466,.F.);
#4669=ADVANCED_FACE('',(#933),#686,.T.);
#4670=ADVANCED_FACE('',(#934,#555),#4467,.F.);
#4671=ADVANCED_FACE('',(#935,#556),#4468,.T.);
#4672=ADVANCED_FACE('',(#936,#557),#687,.T.);
#4673=ADVANCED_FACE('',(#937,#558),#688,.F.);
#4674=ADVANCED_FACE('',(#938),#689,.T.);
#4675=ADVANCED_FACE('',(#939),#4469,.F.);
#4676=ADVANCED_FACE('',(#940),#690,.T.);
#4677=ADVANCED_FACE('',(#941,#559),#4470,.F.);
#4678=ADVANCED_FACE('',(#942,#560),#4471,.T.);
#4679=ADVANCED_FACE('',(#943,#561),#691,.T.);
#4680=ADVANCED_FACE('',(#944,#562),#692,.F.);
#4681=ADVANCED_FACE('',(#945),#693,.F.);
#4682=ADVANCED_FACE('',(#946),#694,.T.);
#4683=ADVANCED_FACE('',(#947),#695,.T.);
#4684=ADVANCED_FACE('',(#948),#696,.T.);
#4685=ADVANCED_FACE('',(#949),#697,.T.);
#4686=ADVANCED_FACE('',(#950),#698,.T.);
#4687=ADVANCED_FACE('',(#951),#699,.F.);
#4688=ADVANCED_FACE('',(#952),#700,.T.);
#4689=ADVANCED_FACE('',(#953),#701,.T.);
#4690=ADVANCED_FACE('',(#954),#702,.T.);
#4691=ADVANCED_FACE('',(#955),#703,.T.);
#4692=ADVANCED_FACE('',(#956),#26,.T.);
#4693=ADVANCED_FACE('',(#957),#4472,.T.);
#4694=ADVANCED_FACE('',(#958),#27,.T.);
#4695=ADVANCED_FACE('',(#959,#563),#704,.T.);
#4696=ADVANCED_FACE('',(#960),#28,.T.);
#4697=ADVANCED_FACE('',(#961),#4473,.T.);
#4698=ADVANCED_FACE('',(#962),#29,.T.);
#4699=ADVANCED_FACE('',(#963),#705,.T.);
#4700=ADVANCED_FACE('',(#964),#706,.F.);
#4701=ADVANCED_FACE('',(#965),#707,.F.);
#4702=ADVANCED_FACE('',(#966),#708,.F.);
#4703=ADVANCED_FACE('',(#967),#709,.F.);
#4704=ADVANCED_FACE('',(#968),#710,.F.);
#4705=ADVANCED_FACE('',(#969),#711,.F.);
#4706=ADVANCED_FACE('',(#970),#712,.F.);
#4707=ADVANCED_FACE('',(#971),#713,.F.);
#4708=ADVANCED_FACE('',(#972),#714,.T.);
#4709=ADVANCED_FACE('',(#973),#30,.T.);
#4710=ADVANCED_FACE('',(#974),#4474,.T.);
#4711=ADVANCED_FACE('',(#975),#31,.T.);
#4712=ADVANCED_FACE('',(#976,#564),#715,.T.);
#4713=ADVANCED_FACE('',(#977),#32,.T.);
#4714=ADVANCED_FACE('',(#978),#4475,.T.);
#4715=ADVANCED_FACE('',(#979),#33,.T.);
#4716=ADVANCED_FACE('',(#980),#716,.T.);
#4717=ADVANCED_FACE('',(#981),#717,.F.);
#4718=ADVANCED_FACE('',(#982),#718,.F.);
#4719=ADVANCED_FACE('',(#983),#719,.F.);
#4720=ADVANCED_FACE('',(#984),#720,.F.);
#4721=ADVANCED_FACE('',(#985),#721,.F.);
#4722=ADVANCED_FACE('',(#986),#722,.F.);
#4723=ADVANCED_FACE('',(#987),#723,.F.);
#4724=ADVANCED_FACE('',(#988),#724,.F.);
#4725=ADVANCED_FACE('',(#989),#4476,.F.);
#4726=ADVANCED_FACE('',(#990),#4477,.T.);
#4727=ADVANCED_FACE('',(#991,#565),#725,.T.);
#4728=ADVANCED_FACE('',(#992,#566),#726,.F.);
#4729=ADVANCED_FACE('',(#993),#34,.T.);
#4730=ADVANCED_FACE('',(#994),#35,.T.);
#4731=ADVANCED_FACE('',(#995),#727,.T.);
#4732=ADVANCED_FACE('',(#996),#728,.T.);
#4733=ADVANCED_FACE('',(#997),#729,.T.);
#4734=ADVANCED_FACE('',(#998),#4478,.F.);
#4735=ADVANCED_FACE('',(#999),#730,.T.);
#4736=ADVANCED_FACE('',(#1000),#731,.T.);
#4737=ADVANCED_FACE('',(#1001),#732,.T.);
#4738=ADVANCED_FACE('',(#1002,#567),#733,.T.);
#4739=ADVANCED_FACE('',(#1003,#568),#734,.F.);
#4740=ADVANCED_FACE('',(#1004),#735,.F.);
#4741=ADVANCED_FACE('',(#1005),#736,.F.);
#4742=ADVANCED_FACE('',(#1006),#737,.F.);
#4743=ADVANCED_FACE('',(#1007),#738,.F.);
#4744=ADVANCED_FACE('',(#1008),#739,.F.);
#4745=ADVANCED_FACE('',(#1009),#740,.F.);
#4746=ADVANCED_FACE('',(#1010),#741,.F.);
#4747=ADVANCED_FACE('',(#1011,#569),#742,.T.);
#4748=ADVANCED_FACE('',(#1012),#36,.T.);
#4749=ADVANCED_FACE('',(#1013),#4479,.T.);
#4750=ADVANCED_FACE('',(#1014),#37,.T.);
#4751=ADVANCED_FACE('',(#1015),#743,.T.);
#4752=CLOSED_SHELL('',(#4480,#4481,#4482,#4483,#4484,#4485,#4486,#4487,
#4488,#4489));
#4753=CLOSED_SHELL('',(#4490,#4491,#4492,#4493,#4494,#4495));
#4754=CLOSED_SHELL('',(#4496,#4497,#4498,#4499,#4500,#4501));
#4755=CLOSED_SHELL('',(#4502,#4503,#4504,#4505,#4506,#4507,#4508,#4509,
#4510,#4511));
#4756=CLOSED_SHELL('',(#4512,#4513,#4514,#4515));
#4757=CLOSED_SHELL('',(#4516,#4517,#4518,#4519));
#4758=CLOSED_SHELL('',(#4520,#4521,#4522,#4523,#4524,#4525,#4526,#4527,
#4528,#4529));
#4759=CLOSED_SHELL('',(#4530,#4531,#4532,#4533));
#4760=CLOSED_SHELL('',(#4534,#4535,#4536,#4537));
#4761=CLOSED_SHELL('',(#4538,#4539,#4540,#4541,#4542,#4543,#4544,#4545,
#4546,#4547,#4548,#4549,#4550,#4551,#4552,#4553,#4554,#4555,#4556,#4557,
#4558,#4559,#4560,#4561,#4562));
#4762=CLOSED_SHELL('',(#4563,#4564,#4565,#4566));
#4763=CLOSED_SHELL('',(#4567,#4568,#4569,#4570,#4571,#4572,#4573,#4574,
#4575,#4576,#4577,#4578));
#4764=CLOSED_SHELL('',(#4579,#4580,#4581,#4582));
#4765=CLOSED_SHELL('',(#4583,#4584,#4585,#4586,#4587,#4588,#4589,#4590));
#4766=CLOSED_SHELL('',(#4591,#4592,#4593,#4594,#4595,#4596,#4597,#4598));
#4767=CLOSED_SHELL('',(#4599,#4600,#4601,#4602,#4603,#4604,#4605,#4606,
#4607,#4608));
#4768=CLOSED_SHELL('',(#4609,#4610,#4611,#4612,#4613,#4614,#4615,#4616,
#4617,#4618,#4619,#4620,#4621,#4622,#4623,#4624,#4625,#4626));
#4769=CLOSED_SHELL('',(#4627,#4628,#4629,#4630));
#4770=CLOSED_SHELL('',(#4631,#4632,#4633,#4634,#4635,#4636,#4637,#4638,
#4639,#4640));
#4771=CLOSED_SHELL('',(#4641,#4642,#4643,#4644,#4645,#4646,#4647,#4648,
#4649,#4650,#4651,#4652,#4653,#4654,#4655,#4656,#4657,#4658));
#4772=CLOSED_SHELL('',(#4659,#4660,#4661,#4662));
#4773=CLOSED_SHELL('',(#4663,#4664,#4665,#4666));
#4774=CLOSED_SHELL('',(#4667,#4668,#4669,#4670,#4671,#4672,#4673));
#4775=CLOSED_SHELL('',(#4674,#4675,#4676,#4677,#4678,#4679,#4680));
#4776=CLOSED_SHELL('',(#4681,#4682,#4683,#4684,#4685,#4686,#4687,#4688,
#4689,#4690));
#4777=CLOSED_SHELL('',(#4691,#4692,#4693,#4694,#4695,#4696,#4697,#4698,
#4699));
#4778=CLOSED_SHELL('',(#4700,#4701,#4702,#4703,#4704,#4705,#4706,#4707));
#4779=CLOSED_SHELL('',(#4708,#4709,#4710,#4711,#4712,#4713,#4714,#4715,
#4716));
#4780=CLOSED_SHELL('',(#4717,#4718,#4719,#4720,#4721,#4722,#4723,#4724));
#4781=CLOSED_SHELL('',(#4725,#4726,#4727,#4728));
#4782=CLOSED_SHELL('',(#4729,#4730,#4731,#4732,#4733,#4734,#4735,#4736,
#4737,#4738,#4739));
#4783=CLOSED_SHELL('',(#4740,#4741,#4742,#4743,#4744,#4745,#4746,#4747,
#4748,#4749,#4750,#4751));
#4784=DERIVED_UNIT_ELEMENT(#4840,1.);
#4785=DERIVED_UNIT_ELEMENT(#9143,-3.);
#4786=DERIVED_UNIT_ELEMENT(#4840,1.);
#4787=DERIVED_UNIT_ELEMENT(#9143,-3.);
#4788=DERIVED_UNIT_ELEMENT(#4840,1.);
#4789=DERIVED_UNIT_ELEMENT(#9143,-3.);
#4790=DERIVED_UNIT_ELEMENT(#4840,1.);
#4791=DERIVED_UNIT_ELEMENT(#9143,-3.);
#4792=DERIVED_UNIT_ELEMENT(#4840,1.);
#4793=DERIVED_UNIT_ELEMENT(#9143,-3.);
#4794=DERIVED_UNIT_ELEMENT(#4840,1.);
#4795=DERIVED_UNIT_ELEMENT(#9143,-3.);
#4796=DERIVED_UNIT_ELEMENT(#4840,1.);
#4797=DERIVED_UNIT_ELEMENT(#9143,-3.);
#4798=DERIVED_UNIT_ELEMENT(#4840,1.);
#4799=DERIVED_UNIT_ELEMENT(#9143,-3.);
#4800=DERIVED_UNIT_ELEMENT(#4840,1.);
#4801=DERIVED_UNIT_ELEMENT(#9143,-3.);
#4802=DERIVED_UNIT_ELEMENT(#4840,1.);
#4803=DERIVED_UNIT_ELEMENT(#9143,-3.);
#4804=DERIVED_UNIT_ELEMENT(#4840,1.);
#4805=DERIVED_UNIT_ELEMENT(#9143,-3.);
#4806=DERIVED_UNIT_ELEMENT(#4840,1.);
#4807=DERIVED_UNIT_ELEMENT(#9143,-3.);
#4808=DERIVED_UNIT_ELEMENT(#4840,1.);
#4809=DERIVED_UNIT_ELEMENT(#9143,-3.);
#4810=DERIVED_UNIT_ELEMENT(#4840,1.);
#4811=DERIVED_UNIT_ELEMENT(#9143,-3.);
#4812=DERIVED_UNIT_ELEMENT(#4840,1.);
#4813=DERIVED_UNIT_ELEMENT(#9143,-3.);
#4814=DERIVED_UNIT_ELEMENT(#4840,1.);
#4815=DERIVED_UNIT_ELEMENT(#9143,-3.);
#4816=DERIVED_UNIT_ELEMENT(#4840,1.);
#4817=DERIVED_UNIT_ELEMENT(#9143,-3.);
#4818=DERIVED_UNIT_ELEMENT(#4840,1.);
#4819=DERIVED_UNIT_ELEMENT(#9143,-3.);
#4820=DERIVED_UNIT_ELEMENT(#4840,1.);
#4821=DERIVED_UNIT_ELEMENT(#9143,-3.);
#4822=DERIVED_UNIT_ELEMENT(#4840,1.);
#4823=DERIVED_UNIT_ELEMENT(#9143,-3.);
#4824=DERIVED_UNIT_ELEMENT(#4840,1.);
#4825=DERIVED_UNIT_ELEMENT(#9143,-3.);
#4826=DERIVED_UNIT_ELEMENT(#4840,1.);
#4827=DERIVED_UNIT_ELEMENT(#9143,-3.);
#4828=DERIVED_UNIT_ELEMENT(#4840,1.);
#4829=DERIVED_UNIT_ELEMENT(#9143,-3.);
#4830=DERIVED_UNIT_ELEMENT(#4840,1.);
#4831=DERIVED_UNIT_ELEMENT(#9143,-3.);
#4832=DERIVED_UNIT_ELEMENT(#4840,1.);
#4833=DERIVED_UNIT_ELEMENT(#9143,-3.);
#4834=DERIVED_UNIT_ELEMENT(#4840,1.);
#4835=DERIVED_UNIT_ELEMENT(#9143,-3.);
#4836=DERIVED_UNIT_ELEMENT(#4840,1.);
#4837=DERIVED_UNIT_ELEMENT(#9143,-3.);
#4838=DERIVED_UNIT_ELEMENT(#4840,1.);
#4839=DERIVED_UNIT_ELEMENT(#9143,-3.);
#4840=(
MASS_UNIT()
NAMED_UNIT(*)
SI_UNIT(.KILO.,.GRAM.)
);
#4841=DERIVED_UNIT((#4784,#4785));
#4842=DERIVED_UNIT((#4786,#4787));
#4843=DERIVED_UNIT((#4788,#4789));
#4844=DERIVED_UNIT((#4790,#4791));
#4845=DERIVED_UNIT((#4792,#4793));
#4846=DERIVED_UNIT((#4794,#4795));
#4847=DERIVED_UNIT((#4796,#4797));
#4848=DERIVED_UNIT((#4798,#4799));
#4849=DERIVED_UNIT((#4800,#4801));
#4850=DERIVED_UNIT((#4802,#4803));
#4851=DERIVED_UNIT((#4804,#4805));
#4852=DERIVED_UNIT((#4806,#4807));
#4853=DERIVED_UNIT((#4808,#4809));
#4854=DERIVED_UNIT((#4810,#4811));
#4855=DERIVED_UNIT((#4812,#4813));
#4856=DERIVED_UNIT((#4814,#4815));
#4857=DERIVED_UNIT((#4816,#4817));
#4858=DERIVED_UNIT((#4818,#4819));
#4859=DERIVED_UNIT((#4820,#4821));
#4860=DERIVED_UNIT((#4822,#4823));
#4861=DERIVED_UNIT((#4824,#4825));
#4862=DERIVED_UNIT((#4826,#4827));
#4863=DERIVED_UNIT((#4828,#4829));
#4864=DERIVED_UNIT((#4830,#4831));
#4865=DERIVED_UNIT((#4832,#4833));
#4866=DERIVED_UNIT((#4834,#4835));
#4867=DERIVED_UNIT((#4836,#4837));
#4868=DERIVED_UNIT((#4838,#4839));
#4869=MEASURE_REPRESENTATION_ITEM('density measure',
POSITIVE_RATIO_MEASURE(7850.),#4841);
#4870=MEASURE_REPRESENTATION_ITEM('density measure',
POSITIVE_RATIO_MEASURE(7850.),#4842);
#4871=MEASURE_REPRESENTATION_ITEM('density measure',
POSITIVE_RATIO_MEASURE(7850.),#4843);
#4872=MEASURE_REPRESENTATION_ITEM('density measure',
POSITIVE_RATIO_MEASURE(7850.),#4844);
#4873=MEASURE_REPRESENTATION_ITEM('density measure',
POSITIVE_RATIO_MEASURE(7850.),#4845);
#4874=MEASURE_REPRESENTATION_ITEM('density measure',
POSITIVE_RATIO_MEASURE(7850.),#4846);
#4875=MEASURE_REPRESENTATION_ITEM('density measure',
POSITIVE_RATIO_MEASURE(7850.),#4847);
#4876=MEASURE_REPRESENTATION_ITEM('density measure',
POSITIVE_RATIO_MEASURE(7850.),#4848);
#4877=MEASURE_REPRESENTATION_ITEM('density measure',
POSITIVE_RATIO_MEASURE(7850.),#4849);
#4878=MEASURE_REPRESENTATION_ITEM('density measure',
POSITIVE_RATIO_MEASURE(7850.),#4850);
#4879=MEASURE_REPRESENTATION_ITEM('density measure',
POSITIVE_RATIO_MEASURE(7850.),#4851);
#4880=MEASURE_REPRESENTATION_ITEM('density measure',
POSITIVE_RATIO_MEASURE(7850.),#4852);
#4881=MEASURE_REPRESENTATION_ITEM('density measure',
POSITIVE_RATIO_MEASURE(7850.),#4853);
#4882=MEASURE_REPRESENTATION_ITEM('density measure',
POSITIVE_RATIO_MEASURE(7850.),#4854);
#4883=MEASURE_REPRESENTATION_ITEM('density measure',
POSITIVE_RATIO_MEASURE(7850.),#4855);
#4884=MEASURE_REPRESENTATION_ITEM('density measure',
POSITIVE_RATIO_MEASURE(7850.),#4856);
#4885=MEASURE_REPRESENTATION_ITEM('density measure',
POSITIVE_RATIO_MEASURE(7850.),#4857);
#4886=MEASURE_REPRESENTATION_ITEM('density measure',
POSITIVE_RATIO_MEASURE(7850.),#4858);
#4887=MEASURE_REPRESENTATION_ITEM('density measure',
POSITIVE_RATIO_MEASURE(7850.),#4859);
#4888=MEASURE_REPRESENTATION_ITEM('density measure',
POSITIVE_RATIO_MEASURE(7850.),#4860);
#4889=MEASURE_REPRESENTATION_ITEM('density measure',
POSITIVE_RATIO_MEASURE(7850.),#4861);
#4890=MEASURE_REPRESENTATION_ITEM('density measure',
POSITIVE_RATIO_MEASURE(7850.),#4862);
#4891=MEASURE_REPRESENTATION_ITEM('density measure',
POSITIVE_RATIO_MEASURE(7850.),#4863);
#4892=MEASURE_REPRESENTATION_ITEM('density measure',
POSITIVE_RATIO_MEASURE(7850.),#4864);
#4893=MEASURE_REPRESENTATION_ITEM('density measure',
POSITIVE_RATIO_MEASURE(7850.),#4865);
#4894=MEASURE_REPRESENTATION_ITEM('density measure',
POSITIVE_RATIO_MEASURE(7850.),#4866);
#4895=MEASURE_REPRESENTATION_ITEM('density measure',
POSITIVE_RATIO_MEASURE(7850.),#4867);
#4896=MEASURE_REPRESENTATION_ITEM('density measure',
POSITIVE_RATIO_MEASURE(7850.),#4868);
#4897=PROPERTY_DEFINITION_REPRESENTATION(#5037,#4953);
#4898=PROPERTY_DEFINITION_REPRESENTATION(#5038,#4954);
#4899=PROPERTY_DEFINITION_REPRESENTATION(#5039,#4955);
#4900=PROPERTY_DEFINITION_REPRESENTATION(#5040,#4956);
#4901=PROPERTY_DEFINITION_REPRESENTATION(#5041,#4957);
#4902=PROPERTY_DEFINITION_REPRESENTATION(#5042,#4958);
#4903=PROPERTY_DEFINITION_REPRESENTATION(#5043,#4959);
#4904=PROPERTY_DEFINITION_REPRESENTATION(#5044,#4960);
#4905=PROPERTY_DEFINITION_REPRESENTATION(#5045,#4961);
#4906=PROPERTY_DEFINITION_REPRESENTATION(#5046,#4962);
#4907=PROPERTY_DEFINITION_REPRESENTATION(#5047,#4963);
#4908=PROPERTY_DEFINITION_REPRESENTATION(#5048,#4964);
#4909=PROPERTY_DEFINITION_REPRESENTATION(#5049,#4965);
#4910=PROPERTY_DEFINITION_REPRESENTATION(#5050,#4966);
#4911=PROPERTY_DEFINITION_REPRESENTATION(#5051,#4967);
#4912=PROPERTY_DEFINITION_REPRESENTATION(#5052,#4968);
#4913=PROPERTY_DEFINITION_REPRESENTATION(#5053,#4969);
#4914=PROPERTY_DEFINITION_REPRESENTATION(#5054,#4970);
#4915=PROPERTY_DEFINITION_REPRESENTATION(#5055,#4971);
#4916=PROPERTY_DEFINITION_REPRESENTATION(#5056,#4972);
#4917=PROPERTY_DEFINITION_REPRESENTATION(#5057,#4973);
#4918=PROPERTY_DEFINITION_REPRESENTATION(#5058,#4974);
#4919=PROPERTY_DEFINITION_REPRESENTATION(#5059,#4975);
#4920=PROPERTY_DEFINITION_REPRESENTATION(#5060,#4976);
#4921=PROPERTY_DEFINITION_REPRESENTATION(#5061,#4977);
#4922=PROPERTY_DEFINITION_REPRESENTATION(#5062,#4978);
#4923=PROPERTY_DEFINITION_REPRESENTATION(#5063,#4979);
#4924=PROPERTY_DEFINITION_REPRESENTATION(#5064,#4980);
#4925=PROPERTY_DEFINITION_REPRESENTATION(#5065,#4981);
#4926=PROPERTY_DEFINITION_REPRESENTATION(#5066,#4982);
#4927=PROPERTY_DEFINITION_REPRESENTATION(#5067,#4983);
#4928=PROPERTY_DEFINITION_REPRESENTATION(#5068,#4984);
#4929=PROPERTY_DEFINITION_REPRESENTATION(#5069,#4985);
#4930=PROPERTY_DEFINITION_REPRESENTATION(#5070,#4986);
#4931=PROPERTY_DEFINITION_REPRESENTATION(#5071,#4987);
#4932=PROPERTY_DEFINITION_REPRESENTATION(#5072,#4988);
#4933=PROPERTY_DEFINITION_REPRESENTATION(#5073,#4989);
#4934=PROPERTY_DEFINITION_REPRESENTATION(#5074,#4990);
#4935=PROPERTY_DEFINITION_REPRESENTATION(#5075,#4991);
#4936=PROPERTY_DEFINITION_REPRESENTATION(#5076,#4992);
#4937=PROPERTY_DEFINITION_REPRESENTATION(#5077,#4993);
#4938=PROPERTY_DEFINITION_REPRESENTATION(#5078,#4994);
#4939=PROPERTY_DEFINITION_REPRESENTATION(#5079,#4995);
#4940=PROPERTY_DEFINITION_REPRESENTATION(#5080,#4996);
#4941=PROPERTY_DEFINITION_REPRESENTATION(#5081,#4997);
#4942=PROPERTY_DEFINITION_REPRESENTATION(#5082,#4998);
#4943=PROPERTY_DEFINITION_REPRESENTATION(#5083,#4999);
#4944=PROPERTY_DEFINITION_REPRESENTATION(#5084,#5000);
#4945=PROPERTY_DEFINITION_REPRESENTATION(#5085,#5001);
#4946=PROPERTY_DEFINITION_REPRESENTATION(#5086,#5002);
#4947=PROPERTY_DEFINITION_REPRESENTATION(#5087,#5003);
#4948=PROPERTY_DEFINITION_REPRESENTATION(#5088,#5004);
#4949=PROPERTY_DEFINITION_REPRESENTATION(#5089,#5005);
#4950=PROPERTY_DEFINITION_REPRESENTATION(#5090,#5006);
#4951=PROPERTY_DEFINITION_REPRESENTATION(#5091,#5007);
#4952=PROPERTY_DEFINITION_REPRESENTATION(#5092,#5008);
#4953=REPRESENTATION('material name',(#5009),#9111);
#4954=REPRESENTATION('density',(#4869),#9111);
#4955=REPRESENTATION('material name',(#5010),#9112);
#4956=REPRESENTATION('density',(#4870),#9112);
#4957=REPRESENTATION('material name',(#5011),#9113);
#4958=REPRESENTATION('density',(#4871),#9113);
#4959=REPRESENTATION('material name',(#5012),#9114);
#4960=REPRESENTATION('density',(#4872),#9114);
#4961=REPRESENTATION('material name',(#5013),#9115);
#4962=REPRESENTATION('density',(#4873),#9115);
#4963=REPRESENTATION('material name',(#5014),#9116);
#4964=REPRESENTATION('density',(#4874),#9116);
#4965=REPRESENTATION('material name',(#5015),#9117);
#4966=REPRESENTATION('density',(#4875),#9117);
#4967=REPRESENTATION('material name',(#5016),#9118);
#4968=REPRESENTATION('density',(#4876),#9118);
#4969=REPRESENTATION('material name',(#5017),#9119);
#4970=REPRESENTATION('density',(#4877),#9119);
#4971=REPRESENTATION('material name',(#5018),#9121);
#4972=REPRESENTATION('density',(#4878),#9121);
#4973=REPRESENTATION('material name',(#5019),#9122);
#4974=REPRESENTATION('density',(#4879),#9122);
#4975=REPRESENTATION('material name',(#5020),#9123);
#4976=REPRESENTATION('density',(#4880),#9123);
#4977=REPRESENTATION('material name',(#5021),#9124);
#4978=REPRESENTATION('density',(#4881),#9124);
#4979=REPRESENTATION('material name',(#5022),#9126);
#4980=REPRESENTATION('density',(#4882),#9126);
#4981=REPRESENTATION('material name',(#5023),#9127);
#4982=REPRESENTATION('density',(#4883),#9127);
#4983=REPRESENTATION('material name',(#5024),#9128);
#4984=REPRESENTATION('density',(#4884),#9128);
#4985=REPRESENTATION('material name',(#5025),#9129);
#4986=REPRESENTATION('density',(#4885),#9129);
#4987=REPRESENTATION('material name',(#5026),#9130);
#4988=REPRESENTATION('density',(#4886),#9130);
#4989=REPRESENTATION('material name',(#5027),#9131);
#4990=REPRESENTATION('density',(#4887),#9131);
#4991=REPRESENTATION('material name',(#5028),#9132);
#4992=REPRESENTATION('density',(#4888),#9132);
#4993=REPRESENTATION('material name',(#5029),#9133);
#4994=REPRESENTATION('density',(#4889),#9133);
#4995=REPRESENTATION('material name',(#5030),#9134);
#4996=REPRESENTATION('density',(#4890),#9134);
#4997=REPRESENTATION('material name',(#5031),#9135);
#4998=REPRESENTATION('density',(#4891),#9135);
#4999=REPRESENTATION('material name',(#5032),#9136);
#5000=REPRESENTATION('density',(#4892),#9136);
#5001=REPRESENTATION('material name',(#5033),#9137);
#5002=REPRESENTATION('density',(#4893),#9137);
#5003=REPRESENTATION('material name',(#5034),#9138);
#5004=REPRESENTATION('density',(#4894),#9138);
#5005=REPRESENTATION('material name',(#5035),#9139);
#5006=REPRESENTATION('density',(#4895),#9139);
#5007=REPRESENTATION('material name',(#5036),#9140);
#5008=REPRESENTATION('density',(#4896),#9140);
#5009=DESCRIPTIVE_REPRESENTATION_ITEM('Steel','Steel');
#5010=DESCRIPTIVE_REPRESENTATION_ITEM('Steel','Steel');
#5011=DESCRIPTIVE_REPRESENTATION_ITEM('Steel','Steel');
#5012=DESCRIPTIVE_REPRESENTATION_ITEM('Steel','Steel');
#5013=DESCRIPTIVE_REPRESENTATION_ITEM('Steel','Steel');
#5014=DESCRIPTIVE_REPRESENTATION_ITEM('Steel','Steel');
#5015=DESCRIPTIVE_REPRESENTATION_ITEM('Steel','Steel');
#5016=DESCRIPTIVE_REPRESENTATION_ITEM('Steel','Steel');
#5017=DESCRIPTIVE_REPRESENTATION_ITEM('Steel','Steel');
#5018=DESCRIPTIVE_REPRESENTATION_ITEM('Steel','Steel');
#5019=DESCRIPTIVE_REPRESENTATION_ITEM('Steel','Steel');
#5020=DESCRIPTIVE_REPRESENTATION_ITEM('Steel','Steel');
#5021=DESCRIPTIVE_REPRESENTATION_ITEM('Steel','Steel');
#5022=DESCRIPTIVE_REPRESENTATION_ITEM('Steel','Steel');
#5023=DESCRIPTIVE_REPRESENTATION_ITEM('Steel','Steel');
#5024=DESCRIPTIVE_REPRESENTATION_ITEM('Steel','Steel');
#5025=DESCRIPTIVE_REPRESENTATION_ITEM('Steel','Steel');
#5026=DESCRIPTIVE_REPRESENTATION_ITEM('Steel','Steel');
#5027=DESCRIPTIVE_REPRESENTATION_ITEM('Steel','Steel');
#5028=DESCRIPTIVE_REPRESENTATION_ITEM('Steel','Steel');
#5029=DESCRIPTIVE_REPRESENTATION_ITEM('Steel','Steel');
#5030=DESCRIPTIVE_REPRESENTATION_ITEM('Steel','Steel');
#5031=DESCRIPTIVE_REPRESENTATION_ITEM('Steel','Steel');
#5032=DESCRIPTIVE_REPRESENTATION_ITEM('Steel','Steel');
#5033=DESCRIPTIVE_REPRESENTATION_ITEM('Steel','Steel');
#5034=DESCRIPTIVE_REPRESENTATION_ITEM('Steel','Steel');
#5035=DESCRIPTIVE_REPRESENTATION_ITEM('Steel','Steel');
#5036=DESCRIPTIVE_REPRESENTATION_ITEM('Steel','Steel');
#5037=PROPERTY_DEFINITION('material property','material name',#9309);
#5038=PROPERTY_DEFINITION('material property','density of part',#9309);
#5039=PROPERTY_DEFINITION('material property','material name',#9310);
#5040=PROPERTY_DEFINITION('material property','density of part',#9310);
#5041=PROPERTY_DEFINITION('material property','material name',#9311);
#5042=PROPERTY_DEFINITION('material property','density of part',#9311);
#5043=PROPERTY_DEFINITION('material property','material name',#9312);
#5044=PROPERTY_DEFINITION('material property','density of part',#9312);
#5045=PROPERTY_DEFINITION('material property','material name',#9313);
#5046=PROPERTY_DEFINITION('material property','density of part',#9313);
#5047=PROPERTY_DEFINITION('material property','material name',#9314);
#5048=PROPERTY_DEFINITION('material property','density of part',#9314);
#5049=PROPERTY_DEFINITION('material property','material name',#9315);
#5050=PROPERTY_DEFINITION('material property','density of part',#9315);
#5051=PROPERTY_DEFINITION('material property','material name',#9316);
#5052=PROPERTY_DEFINITION('material property','density of part',#9316);
#5053=PROPERTY_DEFINITION('material property','material name',#9317);
#5054=PROPERTY_DEFINITION('material property','density of part',#9317);
#5055=PROPERTY_DEFINITION('material property','material name',#9319);
#5056=PROPERTY_DEFINITION('material property','density of part',#9319);
#5057=PROPERTY_DEFINITION('material property','material name',#9320);
#5058=PROPERTY_DEFINITION('material property','density of part',#9320);
#5059=PROPERTY_DEFINITION('material property','material name',#9321);
#5060=PROPERTY_DEFINITION('material property','density of part',#9321);
#5061=PROPERTY_DEFINITION('material property','material name',#9322);
#5062=PROPERTY_DEFINITION('material property','density of part',#9322);
#5063=PROPERTY_DEFINITION('material property','material name',#9324);
#5064=PROPERTY_DEFINITION('material property','density of part',#9324);
#5065=PROPERTY_DEFINITION('material property','material name',#9325);
#5066=PROPERTY_DEFINITION('material property','density of part',#9325);
#5067=PROPERTY_DEFINITION('material property','material name',#9326);
#5068=PROPERTY_DEFINITION('material property','density of part',#9326);
#5069=PROPERTY_DEFINITION('material property','material name',#9327);
#5070=PROPERTY_DEFINITION('material property','density of part',#9327);
#5071=PROPERTY_DEFINITION('material property','material name',#9328);
#5072=PROPERTY_DEFINITION('material property','density of part',#9328);
#5073=PROPERTY_DEFINITION('material property','material name',#9329);
#5074=PROPERTY_DEFINITION('material property','density of part',#9329);
#5075=PROPERTY_DEFINITION('material property','material name',#9330);
#5076=PROPERTY_DEFINITION('material property','density of part',#9330);
#5077=PROPERTY_DEFINITION('material property','material name',#9331);
#5078=PROPERTY_DEFINITION('material property','density of part',#9331);
#5079=PROPERTY_DEFINITION('material property','material name',#9332);
#5080=PROPERTY_DEFINITION('material property','density of part',#9332);
#5081=PROPERTY_DEFINITION('material property','material name',#9333);
#5082=PROPERTY_DEFINITION('material property','density of part',#9333);
#5083=PROPERTY_DEFINITION('material property','material name',#9334);
#5084=PROPERTY_DEFINITION('material property','density of part',#9334);
#5085=PROPERTY_DEFINITION('material property','material name',#9335);
#5086=PROPERTY_DEFINITION('material property','density of part',#9335);
#5087=PROPERTY_DEFINITION('material property','material name',#9336);
#5088=PROPERTY_DEFINITION('material property','density of part',#9336);
#5089=PROPERTY_DEFINITION('material property','material name',#9337);
#5090=PROPERTY_DEFINITION('material property','density of part',#9337);
#5091=PROPERTY_DEFINITION('material property','material name',#9338);
#5092=PROPERTY_DEFINITION('material property','density of part',#9338);
#5093=AXIS2_PLACEMENT_3D('',#7085,#5642,#5643);
#5094=AXIS2_PLACEMENT_3D('',#7086,#5644,#5645);
#5095=AXIS2_PLACEMENT_3D('',#7087,#5646,#5647);
#5096=AXIS2_PLACEMENT_3D('',#7088,#5648,#5649);
#5097=AXIS2_PLACEMENT_3D('',#7090,#5650,#5651);
#5098=AXIS2_PLACEMENT_3D('',#7093,#5653,#5654);
#5099=AXIS2_PLACEMENT_3D('',#7094,#5655,#5656);
#5100=AXIS2_PLACEMENT_3D('',#7096,#5657,#5658);
#5101=AXIS2_PLACEMENT_3D('',#7099,#5660,#5661);
#5102=AXIS2_PLACEMENT_3D('',#7100,#5662,#5663);
#5103=AXIS2_PLACEMENT_3D('',#7102,#5664,#5665);
#5104=AXIS2_PLACEMENT_3D('',#7105,#5667,#5668);
#5105=AXIS2_PLACEMENT_3D('',#7106,#5669,#5670);
#5106=AXIS2_PLACEMENT_3D('',#7108,#5671,#5672);
#5107=AXIS2_PLACEMENT_3D('',#7111,#5674,#5675);
#5108=AXIS2_PLACEMENT_3D('',#7112,#5676,#5677);
#5109=AXIS2_PLACEMENT_3D('',#7121,#5682,#5683);
#5110=AXIS2_PLACEMENT_3D('',#7127,#5687,#5688);
#5111=AXIS2_PLACEMENT_3D('',#7133,#5692,#5693);
#5112=AXIS2_PLACEMENT_3D('',#7136,#5696,#5697);
#5113=AXIS2_PLACEMENT_3D('',#7137,#5698,#5699);
#5114=AXIS2_PLACEMENT_3D('',#7138,#5700,#5701);
#5115=AXIS2_PLACEMENT_3D('',#7139,#5702,#5703);
#5116=AXIS2_PLACEMENT_3D('',#7148,#5708,#5709);
#5117=AXIS2_PLACEMENT_3D('',#7154,#5713,#5714);
#5118=AXIS2_PLACEMENT_3D('',#7160,#5718,#5719);
#5119=AXIS2_PLACEMENT_3D('',#7163,#5722,#5723);
#5120=AXIS2_PLACEMENT_3D('',#7164,#5724,#5725);
#5121=AXIS2_PLACEMENT_3D('',#7165,#5726,#5727);
#5122=AXIS2_PLACEMENT_3D('',#7166,#5728,#5729);
#5123=AXIS2_PLACEMENT_3D('',#7175,#5734,#5735);
#5124=AXIS2_PLACEMENT_3D('',#7181,#5739,#5740);
#5125=AXIS2_PLACEMENT_3D('',#7187,#5744,#5745);
#5126=AXIS2_PLACEMENT_3D('',#7190,#5748,#5749);
#5127=AXIS2_PLACEMENT_3D('',#7191,#5750,#5751);
#5128=AXIS2_PLACEMENT_3D('',#7192,#5752,#5753);
#5129=AXIS2_PLACEMENT_3D('',#7193,#5754,#5755);
#5130=AXIS2_PLACEMENT_3D('',#7195,#5756,#5757);
#5131=AXIS2_PLACEMENT_3D('',#7198,#5759,#5760);
#5132=AXIS2_PLACEMENT_3D('',#7199,#5761,#5762);
#5133=AXIS2_PLACEMENT_3D('',#7201,#5763,#5764);
#5134=AXIS2_PLACEMENT_3D('',#7204,#5766,#5767);
#5135=AXIS2_PLACEMENT_3D('',#7205,#5768,#5769);
#5136=AXIS2_PLACEMENT_3D('',#7207,#5770,#5771);
#5137=AXIS2_PLACEMENT_3D('',#7210,#5773,#5774);
#5138=AXIS2_PLACEMENT_3D('',#7211,#5775,#5776);
#5139=AXIS2_PLACEMENT_3D('',#7213,#5777,#5778);
#5140=AXIS2_PLACEMENT_3D('',#7216,#5780,#5781);
#5141=AXIS2_PLACEMENT_3D('',#7217,#5782,#5783);
#5142=AXIS2_PLACEMENT_3D('',#7226,#5788,#5789);
#5143=AXIS2_PLACEMENT_3D('',#7232,#5793,#5794);
#5144=AXIS2_PLACEMENT_3D('',#7238,#5798,#5799);
#5145=AXIS2_PLACEMENT_3D('',#7241,#5802,#5803);
#5146=AXIS2_PLACEMENT_3D('',#7242,#5804,#5805);
#5147=AXIS2_PLACEMENT_3D('',#7243,#5806,#5807);
#5148=AXIS2_PLACEMENT_3D('',#7244,#5808,#5809);
#5149=AXIS2_PLACEMENT_3D('',#7246,#5810,#5811);
#5150=AXIS2_PLACEMENT_3D('',#7249,#5813,#5814);
#5151=AXIS2_PLACEMENT_3D('',#7250,#5815,#5816);
#5152=AXIS2_PLACEMENT_3D('',#7252,#5817,#5818);
#5153=AXIS2_PLACEMENT_3D('',#7255,#5820,#5821);
#5154=AXIS2_PLACEMENT_3D('',#7256,#5822,#5823);
#5155=AXIS2_PLACEMENT_3D('',#7257,#5824,#5825);
#5156=AXIS2_PLACEMENT_3D('',#7258,#5826,#5827);
#5157=AXIS2_PLACEMENT_3D('',#7259,#5828,#5829);
#5158=AXIS2_PLACEMENT_3D('',#7261,#5830,#5831);
#5159=AXIS2_PLACEMENT_3D('',#7264,#5833,#5834);
#5160=AXIS2_PLACEMENT_3D('',#7265,#5835,#5836);
#5161=AXIS2_PLACEMENT_3D('',#7267,#5837,#5838);
#5162=AXIS2_PLACEMENT_3D('',#7270,#5840,#5841);
#5163=AXIS2_PLACEMENT_3D('',#7271,#5842,#5843);
#5164=AXIS2_PLACEMENT_3D('',#7272,#5844,#5845);
#5165=AXIS2_PLACEMENT_3D('',#7273,#5846,#5847);
#5166=AXIS2_PLACEMENT_3D('',#7274,#5848,#5849);
#5167=AXIS2_PLACEMENT_3D('',#7276,#5850,#5851);
#5168=AXIS2_PLACEMENT_3D('',#7279,#5853,#5854);
#5169=AXIS2_PLACEMENT_3D('',#7280,#5855,#5856);
#5170=AXIS2_PLACEMENT_3D('',#7282,#5857,#5858);
#5171=AXIS2_PLACEMENT_3D('',#7285,#5860,#5861);
#5172=AXIS2_PLACEMENT_3D('',#7286,#5862,#5863);
#5173=AXIS2_PLACEMENT_3D('',#7288,#5864,#5865);
#5174=AXIS2_PLACEMENT_3D('',#7291,#5867,#5868);
#5175=AXIS2_PLACEMENT_3D('',#7292,#5869,#5870);
#5176=AXIS2_PLACEMENT_3D('',#7294,#5871,#5872);
#5177=AXIS2_PLACEMENT_3D('',#7297,#5874,#5875);
#5178=AXIS2_PLACEMENT_3D('',#7298,#5876,#5877);
#5179=AXIS2_PLACEMENT_3D('',#7307,#5882,#5883);
#5180=AXIS2_PLACEMENT_3D('',#7313,#5887,#5888);
#5181=AXIS2_PLACEMENT_3D('',#7319,#5892,#5893);
#5182=AXIS2_PLACEMENT_3D('',#7322,#5896,#5897);
#5183=AXIS2_PLACEMENT_3D('',#7323,#5898,#5899);
#5184=AXIS2_PLACEMENT_3D('',#7324,#5900,#5901);
#5185=AXIS2_PLACEMENT_3D('',#7325,#5902,#5903);
#5186=AXIS2_PLACEMENT_3D('',#7327,#5904,#5905);
#5187=AXIS2_PLACEMENT_3D('',#7330,#5907,#5908);
#5188=AXIS2_PLACEMENT_3D('',#7331,#5909,#5910);
#5189=AXIS2_PLACEMENT_3D('',#7333,#5911,#5912);
#5190=AXIS2_PLACEMENT_3D('',#7336,#5914,#5915);
#5191=AXIS2_PLACEMENT_3D('',#7337,#5916,#5917);
#5192=AXIS2_PLACEMENT_3D('',#7338,#5918,#5919);
#5193=AXIS2_PLACEMENT_3D('',#7339,#5920,#5921);
#5194=AXIS2_PLACEMENT_3D('',#7340,#5922,#5923);
#5195=AXIS2_PLACEMENT_3D('',#7342,#5924,#5925);
#5196=AXIS2_PLACEMENT_3D('',#7345,#5927,#5928);
#5197=AXIS2_PLACEMENT_3D('',#7346,#5929,#5930);
#5198=AXIS2_PLACEMENT_3D('',#7348,#5931,#5932);
#5199=AXIS2_PLACEMENT_3D('',#7351,#5934,#5935);
#5200=AXIS2_PLACEMENT_3D('',#7352,#5936,#5937);
#5201=AXIS2_PLACEMENT_3D('',#7353,#5938,#5939);
#5202=AXIS2_PLACEMENT_3D('',#7354,#5940,#5941);
#5203=AXIS2_PLACEMENT_3D('',#7355,#5942,#5943);
#5204=AXIS2_PLACEMENT_3D('',#7356,#5944,#5945);
#5205=AXIS2_PLACEMENT_3D('',#7358,#5946,#5947);
#5206=AXIS2_PLACEMENT_3D('',#7361,#5949,#5950);
#5207=AXIS2_PLACEMENT_3D('',#7362,#5951,#5952);
#5208=AXIS2_PLACEMENT_3D('',#7364,#5953,#5954);
#5209=AXIS2_PLACEMENT_3D('',#7367,#5956,#5957);
#5210=AXIS2_PLACEMENT_3D('',#7368,#5958,#5959);
#5211=AXIS2_PLACEMENT_3D('',#7371,#5960,#5961);
#5212=AXIS2_PLACEMENT_3D('',#7372,#5962,#5963);
#5213=AXIS2_PLACEMENT_3D('',#7378,#5966,#5967);
#5214=AXIS2_PLACEMENT_3D('',#7379,#5968,#5969);
#5215=AXIS2_PLACEMENT_3D('',#7384,#5971,#5972);
#5216=AXIS2_PLACEMENT_3D('',#7386,#5974,#5975);
#5217=AXIS2_PLACEMENT_3D('',#7391,#5977,#5978);
#5218=AXIS2_PLACEMENT_3D('',#7393,#5980,#5981);
#5219=AXIS2_PLACEMENT_3D('',#7396,#5984,#5985);
#5220=AXIS2_PLACEMENT_3D('',#7402,#5988,#5989);
#5221=AXIS2_PLACEMENT_3D('',#7403,#5990,#5991);
#5222=AXIS2_PLACEMENT_3D('',#7406,#5994,#5995);
#5223=AXIS2_PLACEMENT_3D('',#7416,#6000,#6001);
#5224=AXIS2_PLACEMENT_3D('',#7418,#6002,#6003);
#5225=AXIS2_PLACEMENT_3D('',#7429,#6010,#6011);
#5226=AXIS2_PLACEMENT_3D('',#7430,#6012,#6013);
#5227=AXIS2_PLACEMENT_3D('',#7431,#6014,#6015);
#5228=AXIS2_PLACEMENT_3D('',#7432,#6016,#6017);
#5229=AXIS2_PLACEMENT_3D('',#7433,#6018,#6019);
#5230=AXIS2_PLACEMENT_3D('',#7434,#6020,#6021);
#5231=AXIS2_PLACEMENT_3D('',#7443,#6026,#6027);
#5232=AXIS2_PLACEMENT_3D('',#7449,#6031,#6032);
#5233=AXIS2_PLACEMENT_3D('',#7455,#6036,#6037);
#5234=AXIS2_PLACEMENT_3D('',#7458,#6040,#6041);
#5235=AXIS2_PLACEMENT_3D('',#7459,#6042,#6043);
#5236=AXIS2_PLACEMENT_3D('',#7461,#6044,#6045);
#5237=AXIS2_PLACEMENT_3D('',#7463,#6047,#6048);
#5238=AXIS2_PLACEMENT_3D('',#7465,#6049,#6050);
#5239=AXIS2_PLACEMENT_3D('',#7467,#6052,#6053);
#5240=AXIS2_PLACEMENT_3D('',#7473,#6057,#6058);
#5241=AXIS2_PLACEMENT_3D('',#7477,#6061,#6062);
#5242=AXIS2_PLACEMENT_3D('',#7481,#6065,#6066);
#5243=AXIS2_PLACEMENT_3D('',#7483,#6068,#6069);
#5244=AXIS2_PLACEMENT_3D('',#7484,#6070,#6071);
#5245=AXIS2_PLACEMENT_3D('',#7485,#6072,#6073);
#5246=AXIS2_PLACEMENT_3D('',#7487,#6074,#6075);
#5247=AXIS2_PLACEMENT_3D('',#7490,#6077,#6078);
#5248=AXIS2_PLACEMENT_3D('',#7491,#6079,#6080);
#5249=AXIS2_PLACEMENT_3D('',#7493,#6081,#6082);
#5250=AXIS2_PLACEMENT_3D('',#7494,#6083,#6084);
#5251=AXIS2_PLACEMENT_3D('',#7497,#6085,#6086);
#5252=AXIS2_PLACEMENT_3D('',#7499,#6087,#6088);
#5253=AXIS2_PLACEMENT_3D('',#7500,#6089,#6090);
#5254=AXIS2_PLACEMENT_3D('',#7501,#6091,#6092);
#5255=AXIS2_PLACEMENT_3D('',#7579,#6094,#6095);
#5256=AXIS2_PLACEMENT_3D('',#7657,#6097,#6098);
#5257=AXIS2_PLACEMENT_3D('',#7659,#6099,#6100);
#5258=AXIS2_PLACEMENT_3D('',#7662,#6102,#6103);
#5259=AXIS2_PLACEMENT_3D('',#7827,#6104,#6105);
#5260=AXIS2_PLACEMENT_3D('',#7864,#6107,#6108);
#5261=AXIS2_PLACEMENT_3D('',#7901,#6110,#6111);
#5262=AXIS2_PLACEMENT_3D('',#7938,#6113,#6114);
#5263=AXIS2_PLACEMENT_3D('',#7975,#6116,#6117);
#5264=AXIS2_PLACEMENT_3D('',#7977,#6118,#6119);
#5265=AXIS2_PLACEMENT_3D('',#7978,#6120,#6121);
#5266=AXIS2_PLACEMENT_3D('',#7980,#6122,#6123);
#5267=AXIS2_PLACEMENT_3D('',#7981,#6124,#6125);
#5268=AXIS2_PLACEMENT_3D('',#7983,#6126,#6127);
#5269=AXIS2_PLACEMENT_3D('',#7985,#6129,#6130);
#5270=AXIS2_PLACEMENT_3D('',#7987,#6131,#6132);
#5271=AXIS2_PLACEMENT_3D('',#7988,#6133,#6134);
#5272=AXIS2_PLACEMENT_3D('',#7990,#6136,#6137);
#5273=AXIS2_PLACEMENT_3D('',#7991,#6138,#6139);
#5274=AXIS2_PLACEMENT_3D('',#7992,#6140,#6141);
#5275=AXIS2_PLACEMENT_3D('',#7993,#6142,#6143);
#5276=AXIS2_PLACEMENT_3D('',#7995,#6144,#6145);
#5277=AXIS2_PLACEMENT_3D('',#7998,#6147,#6148);
#5278=AXIS2_PLACEMENT_3D('',#7999,#6149,#6150);
#5279=AXIS2_PLACEMENT_3D('',#8001,#6151,#6152);
#5280=AXIS2_PLACEMENT_3D('',#8004,#6154,#6155);
#5281=AXIS2_PLACEMENT_3D('',#8005,#6156,#6157);
#5282=AXIS2_PLACEMENT_3D('',#8006,#6158,#6159);
#5283=AXIS2_PLACEMENT_3D('',#8007,#6160,#6161);
#5284=AXIS2_PLACEMENT_3D('',#8008,#6162,#6163);
#5285=AXIS2_PLACEMENT_3D('',#8017,#6168,#6169);
#5286=AXIS2_PLACEMENT_3D('',#8023,#6173,#6174);
#5287=AXIS2_PLACEMENT_3D('',#8029,#6178,#6179);
#5288=AXIS2_PLACEMENT_3D('',#8035,#6183,#6184);
#5289=AXIS2_PLACEMENT_3D('',#8041,#6188,#6189);
#5290=AXIS2_PLACEMENT_3D('',#8044,#6192,#6193);
#5291=AXIS2_PLACEMENT_3D('',#8045,#6194,#6195);
#5292=AXIS2_PLACEMENT_3D('',#8046,#6196,#6197);
#5293=AXIS2_PLACEMENT_3D('',#8048,#6198,#6199);
#5294=AXIS2_PLACEMENT_3D('',#8049,#6200,#6201);
#5295=AXIS2_PLACEMENT_3D('',#8051,#6202,#6203);
#5296=AXIS2_PLACEMENT_3D('',#8052,#6204,#6205);
#5297=AXIS2_PLACEMENT_3D('',#8054,#6206,#6207);
#5298=AXIS2_PLACEMENT_3D('',#8056,#6209,#6210);
#5299=AXIS2_PLACEMENT_3D('',#8058,#6211,#6212);
#5300=AXIS2_PLACEMENT_3D('',#8060,#6214,#6215);
#5301=AXIS2_PLACEMENT_3D('',#8062,#6216,#6217);
#5302=AXIS2_PLACEMENT_3D('',#8064,#6219,#6220);
#5303=AXIS2_PLACEMENT_3D('',#8066,#6221,#6222);
#5304=AXIS2_PLACEMENT_3D('',#8067,#6223,#6224);
#5305=AXIS2_PLACEMENT_3D('',#8069,#6225,#6226);
#5306=AXIS2_PLACEMENT_3D('',#8071,#6228,#6229);
#5307=AXIS2_PLACEMENT_3D('',#8073,#6231,#6232);
#5308=AXIS2_PLACEMENT_3D('',#8074,#6233,#6234);
#5309=AXIS2_PLACEMENT_3D('',#8075,#6235,#6236);
#5310=AXIS2_PLACEMENT_3D('',#8077,#6237,#6238);
#5311=AXIS2_PLACEMENT_3D('',#8080,#6240,#6241);
#5312=AXIS2_PLACEMENT_3D('',#8081,#6242,#6243);
#5313=AXIS2_PLACEMENT_3D('',#8082,#6244,#6245);
#5314=AXIS2_PLACEMENT_3D('',#8091,#6250,#6251);
#5315=AXIS2_PLACEMENT_3D('',#8093,#6252,#6253);
#5316=AXIS2_PLACEMENT_3D('',#8097,#6256,#6257);
#5317=AXIS2_PLACEMENT_3D('',#8103,#6261,#6262);
#5318=AXIS2_PLACEMENT_3D('',#8105,#6264,#6265);
#5319=AXIS2_PLACEMENT_3D('',#8106,#6266,#6267);
#5320=AXIS2_PLACEMENT_3D('',#8107,#6268,#6269);
#5321=AXIS2_PLACEMENT_3D('',#8109,#6270,#6271);
#5322=AXIS2_PLACEMENT_3D('',#8112,#6273,#6274);
#5323=AXIS2_PLACEMENT_3D('',#8113,#6275,#6276);
#5324=AXIS2_PLACEMENT_3D('',#8114,#6277,#6278);
#5325=AXIS2_PLACEMENT_3D('',#8115,#6279,#6280);
#5326=AXIS2_PLACEMENT_3D('',#8116,#6281,#6282);
#5327=AXIS2_PLACEMENT_3D('',#8118,#6283,#6284);
#5328=AXIS2_PLACEMENT_3D('',#8121,#6286,#6287);
#5329=AXIS2_PLACEMENT_3D('',#8122,#6288,#6289);
#5330=AXIS2_PLACEMENT_3D('',#8124,#6290,#6291);
#5331=AXIS2_PLACEMENT_3D('',#8127,#6293,#6294);
#5332=AXIS2_PLACEMENT_3D('',#8128,#6295,#6296);
#5333=AXIS2_PLACEMENT_3D('',#8130,#6297,#6298);
#5334=AXIS2_PLACEMENT_3D('',#8133,#6300,#6301);
#5335=AXIS2_PLACEMENT_3D('',#8134,#6302,#6303);
#5336=AXIS2_PLACEMENT_3D('',#8136,#6304,#6305);
#5337=AXIS2_PLACEMENT_3D('',#8139,#6307,#6308);
#5338=AXIS2_PLACEMENT_3D('',#8140,#6309,#6310);
#5339=AXIS2_PLACEMENT_3D('',#8144,#6312,#6313);
#5340=AXIS2_PLACEMENT_3D('',#8145,#6314,#6315);
#5341=AXIS2_PLACEMENT_3D('',#8158,#6316,#6317);
#5342=AXIS2_PLACEMENT_3D('',#8199,#6319,#6320);
#5343=AXIS2_PLACEMENT_3D('',#8210,#6321,#6322);
#5344=AXIS2_PLACEMENT_3D('',#8212,#6324,#6325);
#5345=AXIS2_PLACEMENT_3D('',#8221,#6330,#6331);
#5346=AXIS2_PLACEMENT_3D('',#8227,#6335,#6336);
#5347=AXIS2_PLACEMENT_3D('',#8233,#6340,#6341);
#5348=AXIS2_PLACEMENT_3D('',#8235,#6342,#6343);
#5349=AXIS2_PLACEMENT_3D('',#8236,#6344,#6345);
#5350=AXIS2_PLACEMENT_3D('',#8237,#6346,#6347);
#5351=AXIS2_PLACEMENT_3D('',#8239,#6348,#6349);
#5352=AXIS2_PLACEMENT_3D('',#8242,#6351,#6352);
#5353=AXIS2_PLACEMENT_3D('',#8243,#6353,#6354);
#5354=AXIS2_PLACEMENT_3D('',#8244,#6355,#6356);
#5355=AXIS2_PLACEMENT_3D('',#8245,#6357,#6358);
#5356=AXIS2_PLACEMENT_3D('',#8247,#6359,#6360);
#5357=AXIS2_PLACEMENT_3D('',#8249,#6361,#6362);
#5358=AXIS2_PLACEMENT_3D('',#8250,#6363,#6364);
#5359=AXIS2_PLACEMENT_3D('',#8252,#6365,#6366);
#5360=AXIS2_PLACEMENT_3D('',#8254,#6368,#6369);
#5361=AXIS2_PLACEMENT_3D('',#8255,#6370,#6371);
#5362=AXIS2_PLACEMENT_3D('',#8257,#6373,#6374);
#5363=AXIS2_PLACEMENT_3D('',#8258,#6375,#6376);
#5364=AXIS2_PLACEMENT_3D('',#8259,#6377,#6378);
#5365=AXIS2_PLACEMENT_3D('',#8261,#6379,#6380);
#5366=AXIS2_PLACEMENT_3D('',#8264,#6382,#6383);
#5367=AXIS2_PLACEMENT_3D('',#8265,#6384,#6385);
#5368=AXIS2_PLACEMENT_3D('',#8267,#6386,#6387);
#5369=AXIS2_PLACEMENT_3D('',#8270,#6389,#6390);
#5370=AXIS2_PLACEMENT_3D('',#8271,#6391,#6392);
#5371=AXIS2_PLACEMENT_3D('',#8272,#6393,#6394);
#5372=AXIS2_PLACEMENT_3D('',#8273,#6395,#6396);
#5373=AXIS2_PLACEMENT_3D('',#8274,#6397,#6398);
#5374=AXIS2_PLACEMENT_3D('',#8276,#6399,#6400);
#5375=AXIS2_PLACEMENT_3D('',#8279,#6402,#6403);
#5376=AXIS2_PLACEMENT_3D('',#8280,#6404,#6405);
#5377=AXIS2_PLACEMENT_3D('',#8281,#6406,#6407);
#5378=AXIS2_PLACEMENT_3D('',#8290,#6412,#6413);
#5379=AXIS2_PLACEMENT_3D('',#8292,#6414,#6415);
#5380=AXIS2_PLACEMENT_3D('',#8296,#6418,#6419);
#5381=AXIS2_PLACEMENT_3D('',#8302,#6423,#6424);
#5382=AXIS2_PLACEMENT_3D('',#8304,#6426,#6427);
#5383=AXIS2_PLACEMENT_3D('',#8305,#6428,#6429);
#5384=AXIS2_PLACEMENT_3D('',#8306,#6430,#6431);
#5385=AXIS2_PLACEMENT_3D('',#8308,#6432,#6433);
#5386=AXIS2_PLACEMENT_3D('',#8311,#6435,#6436);
#5387=AXIS2_PLACEMENT_3D('',#8312,#6437,#6438);
#5388=AXIS2_PLACEMENT_3D('',#8313,#6439,#6440);
#5389=AXIS2_PLACEMENT_3D('',#8314,#6441,#6442);
#5390=AXIS2_PLACEMENT_3D('',#8315,#6443,#6444);
#5391=AXIS2_PLACEMENT_3D('',#8317,#6445,#6446);
#5392=AXIS2_PLACEMENT_3D('',#8320,#6448,#6449);
#5393=AXIS2_PLACEMENT_3D('',#8321,#6450,#6451);
#5394=AXIS2_PLACEMENT_3D('',#8323,#6452,#6453);
#5395=AXIS2_PLACEMENT_3D('',#8326,#6455,#6456);
#5396=AXIS2_PLACEMENT_3D('',#8327,#6457,#6458);
#5397=AXIS2_PLACEMENT_3D('',#8329,#6459,#6460);
#5398=AXIS2_PLACEMENT_3D('',#8332,#6462,#6463);
#5399=AXIS2_PLACEMENT_3D('',#8333,#6464,#6465);
#5400=AXIS2_PLACEMENT_3D('',#8335,#6466,#6467);
#5401=AXIS2_PLACEMENT_3D('',#8338,#6469,#6470);
#5402=AXIS2_PLACEMENT_3D('',#8339,#6471,#6472);
#5403=AXIS2_PLACEMENT_3D('',#8343,#6474,#6475);
#5404=AXIS2_PLACEMENT_3D('',#8344,#6476,#6477);
#5405=AXIS2_PLACEMENT_3D('',#8357,#6478,#6479);
#5406=AXIS2_PLACEMENT_3D('',#8398,#6481,#6482);
#5407=AXIS2_PLACEMENT_3D('',#8409,#6483,#6484);
#5408=AXIS2_PLACEMENT_3D('',#8411,#6486,#6487);
#5409=AXIS2_PLACEMENT_3D('',#8420,#6492,#6493);
#5410=AXIS2_PLACEMENT_3D('',#8429,#6498,#6499);
#5411=AXIS2_PLACEMENT_3D('',#8432,#6502,#6503);
#5412=AXIS2_PLACEMENT_3D('',#8434,#6504,#6505);
#5413=AXIS2_PLACEMENT_3D('',#8435,#6506,#6507);
#5414=AXIS2_PLACEMENT_3D('',#8436,#6508,#6509);
#5415=AXIS2_PLACEMENT_3D('',#8437,#6510,#6511);
#5416=AXIS2_PLACEMENT_3D('',#8438,#6512,#6513);
#5417=AXIS2_PLACEMENT_3D('',#8440,#6514,#6515);
#5418=AXIS2_PLACEMENT_3D('',#8442,#6517,#6518);
#5419=AXIS2_PLACEMENT_3D('',#8444,#6519,#6520);
#5420=AXIS2_PLACEMENT_3D('',#8446,#6521,#6522);
#5421=AXIS2_PLACEMENT_3D('',#8447,#6523,#6524);
#5422=AXIS2_PLACEMENT_3D('',#8450,#6526,#6527);
#5423=AXIS2_PLACEMENT_3D('',#8451,#6528,#6529);
#5424=AXIS2_PLACEMENT_3D('',#8453,#6530,#6531);
#5425=AXIS2_PLACEMENT_3D('',#8455,#6533,#6534);
#5426=AXIS2_PLACEMENT_3D('',#8456,#6535,#6536);
#5427=AXIS2_PLACEMENT_3D('',#8457,#6537,#6538);
#5428=AXIS2_PLACEMENT_3D('',#8458,#6539,#6540);
#5429=AXIS2_PLACEMENT_3D('',#8460,#6541,#6542);
#5430=AXIS2_PLACEMENT_3D('',#8463,#6544,#6545);
#5431=AXIS2_PLACEMENT_3D('',#8464,#6546,#6547);
#5432=AXIS2_PLACEMENT_3D('',#8466,#6548,#6549);
#5433=AXIS2_PLACEMENT_3D('',#8469,#6551,#6552);
#5434=AXIS2_PLACEMENT_3D('',#8470,#6553,#6554);
#5435=AXIS2_PLACEMENT_3D('',#8471,#6555,#6556);
#5436=AXIS2_PLACEMENT_3D('',#8472,#6557,#6558);
#5437=AXIS2_PLACEMENT_3D('',#8473,#6559,#6560);
#5438=AXIS2_PLACEMENT_3D('',#8475,#6561,#6562);
#5439=AXIS2_PLACEMENT_3D('',#8478,#6564,#6565);
#5440=AXIS2_PLACEMENT_3D('',#8479,#6566,#6567);
#5441=AXIS2_PLACEMENT_3D('',#8481,#6568,#6569);
#5442=AXIS2_PLACEMENT_3D('',#8484,#6571,#6572);
#5443=AXIS2_PLACEMENT_3D('',#8485,#6573,#6574);
#5444=AXIS2_PLACEMENT_3D('',#8486,#6575,#6576);
#5445=AXIS2_PLACEMENT_3D('',#8487,#6577,#6578);
#5446=AXIS2_PLACEMENT_3D('',#8488,#6579,#6580);
#5447=AXIS2_PLACEMENT_3D('',#8492,#6582,#6583);
#5448=AXIS2_PLACEMENT_3D('',#8493,#6584,#6585);
#5449=AXIS2_PLACEMENT_3D('',#8510,#6586,#6587);
#5450=AXIS2_PLACEMENT_3D('',#8551,#6589,#6590);
#5451=AXIS2_PLACEMENT_3D('',#8566,#6591,#6592);
#5452=AXIS2_PLACEMENT_3D('',#8568,#6594,#6595);
#5453=AXIS2_PLACEMENT_3D('',#8570,#6596,#6597);
#5454=AXIS2_PLACEMENT_3D('',#8573,#6599,#6600);
#5455=AXIS2_PLACEMENT_3D('',#8574,#6601,#6602);
#5456=AXIS2_PLACEMENT_3D('',#8576,#6603,#6604);
#5457=AXIS2_PLACEMENT_3D('',#8579,#6606,#6607);
#5458=AXIS2_PLACEMENT_3D('',#8580,#6608,#6609);
#5459=AXIS2_PLACEMENT_3D('',#8581,#6610,#6611);
#5460=AXIS2_PLACEMENT_3D('',#8582,#6612,#6613);
#5461=AXIS2_PLACEMENT_3D('',#8583,#6614,#6615);
#5462=AXIS2_PLACEMENT_3D('',#8587,#6617,#6618);
#5463=AXIS2_PLACEMENT_3D('',#8588,#6619,#6620);
#5464=AXIS2_PLACEMENT_3D('',#8605,#6621,#6622);
#5465=AXIS2_PLACEMENT_3D('',#8646,#6624,#6625);
#5466=AXIS2_PLACEMENT_3D('',#8661,#6626,#6627);
#5467=AXIS2_PLACEMENT_3D('',#8663,#6629,#6630);
#5468=AXIS2_PLACEMENT_3D('',#8665,#6631,#6632);
#5469=AXIS2_PLACEMENT_3D('',#8668,#6634,#6635);
#5470=AXIS2_PLACEMENT_3D('',#8669,#6636,#6637);
#5471=AXIS2_PLACEMENT_3D('',#8671,#6638,#6639);
#5472=AXIS2_PLACEMENT_3D('',#8674,#6641,#6642);
#5473=AXIS2_PLACEMENT_3D('',#8675,#6643,#6644);
#5474=AXIS2_PLACEMENT_3D('',#8676,#6645,#6646);
#5475=AXIS2_PLACEMENT_3D('',#8677,#6647,#6648);
#5476=AXIS2_PLACEMENT_3D('',#8678,#6649,#6650);
#5477=AXIS2_PLACEMENT_3D('',#8695,#6659,#6660);
#5478=AXIS2_PLACEMENT_3D('',#8701,#6664,#6665);
#5479=AXIS2_PLACEMENT_3D('',#8705,#6668,#6669);
#5480=AXIS2_PLACEMENT_3D('',#8709,#6672,#6673);
#5481=AXIS2_PLACEMENT_3D('',#8713,#6676,#6677);
#5482=AXIS2_PLACEMENT_3D('',#8721,#6682,#6683);
#5483=AXIS2_PLACEMENT_3D('',#8723,#6685,#6686);
#5484=AXIS2_PLACEMENT_3D('',#8725,#6688,#6689);
#5485=AXIS2_PLACEMENT_3D('',#8727,#6691,#6692);
#5486=AXIS2_PLACEMENT_3D('',#8728,#6693,#6694);
#5487=AXIS2_PLACEMENT_3D('',#8729,#6695,#6696);
#5488=AXIS2_PLACEMENT_3D('',#8731,#6697,#6698);
#5489=AXIS2_PLACEMENT_3D('',#8732,#6699,#6700);
#5490=AXIS2_PLACEMENT_3D('',#8734,#6701,#6702);
#5491=AXIS2_PLACEMENT_3D('',#8736,#6704,#6705);
#5492=AXIS2_PLACEMENT_3D('',#8738,#6706,#6707);
#5493=AXIS2_PLACEMENT_3D('',#8740,#6709,#6710);
#5494=AXIS2_PLACEMENT_3D('',#8742,#6711,#6712);
#5495=AXIS2_PLACEMENT_3D('',#8744,#6714,#6715);
#5496=AXIS2_PLACEMENT_3D('',#8746,#6716,#6717);
#5497=AXIS2_PLACEMENT_3D('',#8747,#6718,#6719);
#5498=AXIS2_PLACEMENT_3D('',#8749,#6720,#6721);
#5499=AXIS2_PLACEMENT_3D('',#8751,#6723,#6724);
#5500=AXIS2_PLACEMENT_3D('',#8753,#6725,#6726);
#5501=AXIS2_PLACEMENT_3D('',#8755,#6728,#6729);
#5502=AXIS2_PLACEMENT_3D('',#8757,#6730,#6731);
#5503=AXIS2_PLACEMENT_3D('',#8759,#6733,#6734);
#5504=AXIS2_PLACEMENT_3D('',#8760,#6735,#6736);
#5505=AXIS2_PLACEMENT_3D('',#8769,#6741,#6742);
#5506=AXIS2_PLACEMENT_3D('',#8775,#6746,#6747);
#5507=AXIS2_PLACEMENT_3D('',#8781,#6751,#6752);
#5508=AXIS2_PLACEMENT_3D('',#8787,#6756,#6757);
#5509=AXIS2_PLACEMENT_3D('',#8793,#6761,#6762);
#5510=AXIS2_PLACEMENT_3D('',#8796,#6765,#6766);
#5511=AXIS2_PLACEMENT_3D('',#8797,#6767,#6768);
#5512=AXIS2_PLACEMENT_3D('',#8798,#6769,#6770);
#5513=AXIS2_PLACEMENT_3D('',#8799,#6771,#6772);
#5514=AXIS2_PLACEMENT_3D('',#8801,#6773,#6774);
#5515=AXIS2_PLACEMENT_3D('',#8802,#6775,#6776);
#5516=AXIS2_PLACEMENT_3D('',#8804,#6777,#6778);
#5517=AXIS2_PLACEMENT_3D('',#8806,#6780,#6781);
#5518=AXIS2_PLACEMENT_3D('',#8808,#6782,#6783);
#5519=AXIS2_PLACEMENT_3D('',#8810,#6785,#6786);
#5520=AXIS2_PLACEMENT_3D('',#8812,#6787,#6788);
#5521=AXIS2_PLACEMENT_3D('',#8814,#6790,#6791);
#5522=AXIS2_PLACEMENT_3D('',#8816,#6792,#6793);
#5523=AXIS2_PLACEMENT_3D('',#8817,#6794,#6795);
#5524=AXIS2_PLACEMENT_3D('',#8819,#6796,#6797);
#5525=AXIS2_PLACEMENT_3D('',#8821,#6799,#6800);
#5526=AXIS2_PLACEMENT_3D('',#8823,#6801,#6802);
#5527=AXIS2_PLACEMENT_3D('',#8825,#6804,#6805);
#5528=AXIS2_PLACEMENT_3D('',#8827,#6806,#6807);
#5529=AXIS2_PLACEMENT_3D('',#8829,#6809,#6810);
#5530=AXIS2_PLACEMENT_3D('',#8830,#6811,#6812);
#5531=AXIS2_PLACEMENT_3D('',#8839,#6817,#6818);
#5532=AXIS2_PLACEMENT_3D('',#8845,#6822,#6823);
#5533=AXIS2_PLACEMENT_3D('',#8851,#6827,#6828);
#5534=AXIS2_PLACEMENT_3D('',#8857,#6832,#6833);
#5535=AXIS2_PLACEMENT_3D('',#8863,#6837,#6838);
#5536=AXIS2_PLACEMENT_3D('',#8866,#6841,#6842);
#5537=AXIS2_PLACEMENT_3D('',#8867,#6843,#6844);
#5538=AXIS2_PLACEMENT_3D('',#8868,#6845,#6846);
#5539=AXIS2_PLACEMENT_3D('',#8869,#6847,#6848);
#5540=AXIS2_PLACEMENT_3D('',#8871,#6849,#6850);
#5541=AXIS2_PLACEMENT_3D('',#8874,#6852,#6853);
#5542=AXIS2_PLACEMENT_3D('',#8875,#6854,#6855);
#5543=AXIS2_PLACEMENT_3D('',#8877,#6856,#6857);
#5544=AXIS2_PLACEMENT_3D('',#8880,#6859,#6860);
#5545=AXIS2_PLACEMENT_3D('',#8881,#6861,#6862);
#5546=AXIS2_PLACEMENT_3D('',#8882,#6863,#6864);
#5547=AXIS2_PLACEMENT_3D('',#8883,#6865,#6866);
#5548=AXIS2_PLACEMENT_3D('',#8884,#6867,#6868);
#5549=AXIS2_PLACEMENT_3D('',#8885,#6869,#6870);
#5550=AXIS2_PLACEMENT_3D('',#8886,#6871,#6872);
#5551=AXIS2_PLACEMENT_3D('',#8887,#6873,#6874);
#5552=AXIS2_PLACEMENT_3D('',#8888,#6875,#6876);
#5553=AXIS2_PLACEMENT_3D('',#8889,#6877,#6878);
#5554=AXIS2_PLACEMENT_3D('',#8890,#6879,#6880);
#5555=AXIS2_PLACEMENT_3D('',#8891,#6881,#6882);
#5556=AXIS2_PLACEMENT_3D('',#8892,#6883,#6884);
#5557=AXIS2_PLACEMENT_3D('',#8893,#6885,#6886);
#5558=AXIS2_PLACEMENT_3D('',#8894,#6887,#6888);
#5559=AXIS2_PLACEMENT_3D('',#8895,#6889,#6890);
#5560=AXIS2_PLACEMENT_3D('',#8896,#6891,#6892);
#5561=AXIS2_PLACEMENT_3D('',#8897,#6893,#6894);
#5562=AXIS2_PLACEMENT_3D('',#8898,#6895,#6896);
#5563=AXIS2_PLACEMENT_3D('',#8899,#6897,#6898);
#5564=AXIS2_PLACEMENT_3D('',#8900,#6899,#6900);
#5565=AXIS2_PLACEMENT_3D('',#8901,#6901,#6902);
#5566=AXIS2_PLACEMENT_3D('',#8902,#6903,#6904);
#5567=AXIS2_PLACEMENT_3D('',#8903,#6905,#6906);
#5568=AXIS2_PLACEMENT_3D('',#8904,#6907,#6908);
#5569=AXIS2_PLACEMENT_3D('',#8905,#6909,#6910);
#5570=AXIS2_PLACEMENT_3D('',#8906,#6911,#6912);
#5571=AXIS2_PLACEMENT_3D('',#8907,#6913,#6914);
#5572=AXIS2_PLACEMENT_3D('',#8908,#6915,#6916);
#5573=AXIS2_PLACEMENT_3D('',#8909,#6917,#6918);
#5574=AXIS2_PLACEMENT_3D('',#8910,#6919,#6920);
#5575=AXIS2_PLACEMENT_3D('',#8911,#6921,#6922);
#5576=AXIS2_PLACEMENT_3D('',#8923,#6924,#6925);
#5577=AXIS2_PLACEMENT_3D('',#8939,#6926,#6927);
#5578=AXIS2_PLACEMENT_3D('',#8941,#6928,#6929);
#5579=AXIS2_PLACEMENT_3D('',#8967,#6931,#6932);
#5580=AXIS2_PLACEMENT_3D('',#8970,#6935,#6936);
#5581=AXIS2_PLACEMENT_3D('',#8972,#6938,#6939);
#5582=AXIS2_PLACEMENT_3D('',#8974,#6941,#6942);
#5583=AXIS2_PLACEMENT_3D('',#8976,#6943,#6944);
#5584=AXIS2_PLACEMENT_3D('',#8979,#6946,#6947);
#5585=AXIS2_PLACEMENT_3D('',#8980,#6948,#6949);
#5586=AXIS2_PLACEMENT_3D('',#8982,#6951,#6952);
#5587=AXIS2_PLACEMENT_3D('',#8984,#6954,#6955);
#5588=AXIS2_PLACEMENT_3D('',#8985,#6956,#6957);
#5589=AXIS2_PLACEMENT_3D('',#8986,#6958,#6959);
#5590=AXIS2_PLACEMENT_3D('',#8987,#6960,#6961);
#5591=AXIS2_PLACEMENT_3D('',#8988,#6962,#6963);
#5592=AXIS2_PLACEMENT_3D('',#8997,#6968,#6969);
#5593=AXIS2_PLACEMENT_3D('',#9003,#6973,#6974);
#5594=AXIS2_PLACEMENT_3D('',#9009,#6978,#6979);
#5595=AXIS2_PLACEMENT_3D('',#9015,#6983,#6984);
#5596=AXIS2_PLACEMENT_3D('',#9021,#6988,#6989);
#5597=AXIS2_PLACEMENT_3D('',#9024,#6992,#6993);
#5598=AXIS2_PLACEMENT_3D('',#9025,#6994,#6995);
#5599=AXIS2_PLACEMENT_3D('',#9027,#6996,#6997);
#5600=AXIS2_PLACEMENT_3D('',#9028,#6998,#6999);
#5601=AXIS2_PLACEMENT_3D('',#9030,#7000,#7001);
#5602=AXIS2_PLACEMENT_3D('',#9032,#7003,#7004);
#5603=AXIS2_PLACEMENT_3D('',#9034,#7005,#7006);
#5604=AXIS2_PLACEMENT_3D('',#9036,#7008,#7009);
#5605=AXIS2_PLACEMENT_3D('',#9038,#7010,#7011);
#5606=AXIS2_PLACEMENT_3D('',#9040,#7013,#7014);
#5607=AXIS2_PLACEMENT_3D('',#9041,#7015,#7016);
#5608=AXIS2_PLACEMENT_3D('',#9042,#7017,#7018);
#5609=AXIS2_PLACEMENT_3D('',#9043,#7019,#7020);
#5610=AXIS2_PLACEMENT_3D('',#9044,#7021,#7022);
#5611=AXIS2_PLACEMENT_3D('',#9045,#7023,#7024);
#5612=AXIS2_PLACEMENT_3D('',#9046,#7025,#7026);
#5613=AXIS2_PLACEMENT_3D('',#9047,#7027,#7028);
#5614=AXIS2_PLACEMENT_3D('',#9048,#7029,#7030);
#5615=AXIS2_PLACEMENT_3D('',#9049,#7031,#7032);
#5616=AXIS2_PLACEMENT_3D('',#9050,#7033,#7034);
#5617=AXIS2_PLACEMENT_3D('',#9051,#7035,#7036);
#5618=AXIS2_PLACEMENT_3D('',#9052,#7037,#7038);
#5619=AXIS2_PLACEMENT_3D('',#9053,#7039,#7040);
#5620=AXIS2_PLACEMENT_3D('',#9054,#7041,#7042);
#5621=AXIS2_PLACEMENT_3D('',#9055,#7043,#7044);
#5622=AXIS2_PLACEMENT_3D('',#9056,#7045,#7046);
#5623=AXIS2_PLACEMENT_3D('',#9057,#7047,#7048);
#5624=AXIS2_PLACEMENT_3D('',#9058,#7049,#7050);
#5625=AXIS2_PLACEMENT_3D('',#9059,#7051,#7052);
#5626=AXIS2_PLACEMENT_3D('',#9060,#7053,#7054);
#5627=AXIS2_PLACEMENT_3D('',#9061,#7055,#7056);
#5628=AXIS2_PLACEMENT_3D('',#9062,#7057,#7058);
#5629=AXIS2_PLACEMENT_3D('',#9063,#7059,#7060);
#5630=AXIS2_PLACEMENT_3D('',#9064,#7061,#7062);
#5631=AXIS2_PLACEMENT_3D('',#9065,#7063,#7064);
#5632=AXIS2_PLACEMENT_3D('',#9066,#7065,#7066);
#5633=AXIS2_PLACEMENT_3D('',#9067,#7067,#7068);
#5634=AXIS2_PLACEMENT_3D('',#9068,#7069,#7070);
#5635=AXIS2_PLACEMENT_3D('',#9069,#7071,#7072);
#5636=AXIS2_PLACEMENT_3D('',#9070,#7073,#7074);
#5637=AXIS2_PLACEMENT_3D('',#9071,#7075,#7076);
#5638=AXIS2_PLACEMENT_3D('',#9072,#7077,#7078);
#5639=AXIS2_PLACEMENT_3D('',#9073,#7079,#7080);
#5640=AXIS2_PLACEMENT_3D('',#9074,#7081,#7082);
#5641=AXIS2_PLACEMENT_3D('',#9075,#7083,#7084);
#5642=DIRECTION('axis',(0.,0.,1.));
#5643=DIRECTION('refdir',(1.,0.,0.));
#5644=DIRECTION('axis',(0.,0.,1.));
#5645=DIRECTION('refdir',(1.,0.,0.));
#5646=DIRECTION('axis',(0.,0.,1.));
#5647=DIRECTION('refdir',(1.,0.,0.));
#5648=DIRECTION('center_axis',(0.,0.,1.));
#5649=DIRECTION('ref_axis',(1.,0.,0.));
#5650=DIRECTION('center_axis',(0.,0.,1.));
#5651=DIRECTION('ref_axis',(1.,0.,0.));
#5652=DIRECTION('',(0.,0.,1.));
#5653=DIRECTION('center_axis',(0.,0.,-1.));
#5654=DIRECTION('ref_axis',(1.,0.,0.));
#5655=DIRECTION('center_axis',(0.,0.,1.));
#5656=DIRECTION('ref_axis',(1.,0.,0.));
#5657=DIRECTION('center_axis',(0.,0.,1.));
#5658=DIRECTION('ref_axis',(1.,0.,0.));
#5659=DIRECTION('',(0.,0.,1.));
#5660=DIRECTION('center_axis',(0.,0.,-1.));
#5661=DIRECTION('ref_axis',(1.,0.,0.));
#5662=DIRECTION('center_axis',(0.,0.,1.));
#5663=DIRECTION('ref_axis',(1.,0.,0.));
#5664=DIRECTION('center_axis',(0.,0.,1.));
#5665=DIRECTION('ref_axis',(1.,0.,0.));
#5666=DIRECTION('',(0.,0.,1.));
#5667=DIRECTION('center_axis',(0.,0.,-1.));
#5668=DIRECTION('ref_axis',(1.,0.,0.));
#5669=DIRECTION('center_axis',(0.,0.,1.));
#5670=DIRECTION('ref_axis',(1.,0.,0.));
#5671=DIRECTION('center_axis',(0.,0.,1.));
#5672=DIRECTION('ref_axis',(1.,0.,0.));
#5673=DIRECTION('',(0.,0.,1.));
#5674=DIRECTION('center_axis',(0.,0.,-1.));
#5675=DIRECTION('ref_axis',(1.,0.,0.));
#5676=DIRECTION('center_axis',(0.,1.,0.));
#5677=DIRECTION('ref_axis',(-1.,0.,0.));
#5678=DIRECTION('',(-1.,0.,0.));
#5679=DIRECTION('',(0.,0.,1.));
#5680=DIRECTION('',(-1.,0.,0.));
#5681=DIRECTION('',(0.,0.,1.));
#5682=DIRECTION('center_axis',(1.,0.,0.));
#5683=DIRECTION('ref_axis',(0.,1.,0.));
#5684=DIRECTION('',(0.,1.,0.));
#5685=DIRECTION('',(0.,1.,0.));
#5686=DIRECTION('',(0.,0.,1.));
#5687=DIRECTION('center_axis',(0.,-1.,0.));
#5688=DIRECTION('ref_axis',(1.,0.,0.));
#5689=DIRECTION('',(1.,0.,0.));
#5690=DIRECTION('',(1.,0.,0.));
#5691=DIRECTION('',(0.,0.,1.));
#5692=DIRECTION('center_axis',(-1.,0.,0.));
#5693=DIRECTION('ref_axis',(0.,-1.,0.));
#5694=DIRECTION('',(0.,-1.,0.));
#5695=DIRECTION('',(0.,-1.,0.));
#5696=DIRECTION('center_axis',(0.,0.,1.));
#5697=DIRECTION('ref_axis',(1.,0.,0.));
#5698=DIRECTION('center_axis',(0.,0.,1.));
#5699=DIRECTION('ref_axis',(1.,0.,0.));
#5700=DIRECTION('axis',(0.,0.,1.));
#5701=DIRECTION('refdir',(1.,0.,0.));
#5702=DIRECTION('center_axis',(0.,1.,0.));
#5703=DIRECTION('ref_axis',(-1.,0.,0.));
#5704=DIRECTION('',(-1.,0.,0.));
#5705=DIRECTION('',(0.,0.,1.));
#5706=DIRECTION('',(-1.,0.,0.));
#5707=DIRECTION('',(0.,0.,1.));
#5708=DIRECTION('center_axis',(1.,0.,0.));
#5709=DIRECTION('ref_axis',(0.,1.,0.));
#5710=DIRECTION('',(0.,1.,0.));
#5711=DIRECTION('',(0.,1.,0.));
#5712=DIRECTION('',(0.,0.,1.));
#5713=DIRECTION('center_axis',(0.,-1.,0.));
#5714=DIRECTION('ref_axis',(1.,0.,0.));
#5715=DIRECTION('',(1.,0.,0.));
#5716=DIRECTION('',(1.,0.,0.));
#5717=DIRECTION('',(0.,0.,1.));
#5718=DIRECTION('center_axis',(-1.,0.,0.));
#5719=DIRECTION('ref_axis',(0.,-1.,0.));
#5720=DIRECTION('',(0.,-1.,0.));
#5721=DIRECTION('',(0.,-1.,0.));
#5722=DIRECTION('center_axis',(0.,0.,1.));
#5723=DIRECTION('ref_axis',(1.,0.,0.));
#5724=DIRECTION('center_axis',(0.,0.,1.));
#5725=DIRECTION('ref_axis',(1.,0.,0.));
#5726=DIRECTION('axis',(0.,0.,1.));
#5727=DIRECTION('refdir',(1.,0.,0.));
#5728=DIRECTION('center_axis',(0.,1.,0.));
#5729=DIRECTION('ref_axis',(-1.,0.,0.));
#5730=DIRECTION('',(-1.,0.,0.));
#5731=DIRECTION('',(0.,0.,1.));
#5732=DIRECTION('',(-1.,0.,0.));
#5733=DIRECTION('',(0.,0.,1.));
#5734=DIRECTION('center_axis',(1.,0.,0.));
#5735=DIRECTION('ref_axis',(0.,1.,0.));
#5736=DIRECTION('',(0.,1.,0.));
#5737=DIRECTION('',(0.,1.,0.));
#5738=DIRECTION('',(0.,0.,1.));
#5739=DIRECTION('center_axis',(0.,-1.,0.));
#5740=DIRECTION('ref_axis',(1.,0.,0.));
#5741=DIRECTION('',(1.,0.,0.));
#5742=DIRECTION('',(1.,0.,0.));
#5743=DIRECTION('',(0.,0.,1.));
#5744=DIRECTION('center_axis',(-1.,0.,0.));
#5745=DIRECTION('ref_axis',(0.,-1.,0.));
#5746=DIRECTION('',(0.,-1.,0.));
#5747=DIRECTION('',(0.,-1.,0.));
#5748=DIRECTION('center_axis',(0.,0.,1.));
#5749=DIRECTION('ref_axis',(1.,0.,0.));
#5750=DIRECTION('center_axis',(0.,0.,1.));
#5751=DIRECTION('ref_axis',(1.,0.,0.));
#5752=DIRECTION('axis',(0.,0.,1.));
#5753=DIRECTION('refdir',(1.,0.,0.));
#5754=DIRECTION('center_axis',(0.,0.,1.));
#5755=DIRECTION('ref_axis',(1.,0.,0.));
#5756=DIRECTION('center_axis',(0.,0.,1.));
#5757=DIRECTION('ref_axis',(1.,0.,0.));
#5758=DIRECTION('',(0.,0.,1.));
#5759=DIRECTION('center_axis',(0.,0.,-1.));
#5760=DIRECTION('ref_axis',(1.,0.,0.));
#5761=DIRECTION('center_axis',(0.,0.,1.));
#5762=DIRECTION('ref_axis',(1.,0.,0.));
#5763=DIRECTION('center_axis',(0.,0.,1.));
#5764=DIRECTION('ref_axis',(1.,0.,0.));
#5765=DIRECTION('',(0.,0.,1.));
#5766=DIRECTION('center_axis',(0.,0.,-1.));
#5767=DIRECTION('ref_axis',(1.,0.,0.));
#5768=DIRECTION('center_axis',(0.,0.,1.));
#5769=DIRECTION('ref_axis',(1.,0.,0.));
#5770=DIRECTION('center_axis',(0.,0.,1.));
#5771=DIRECTION('ref_axis',(1.,0.,0.));
#5772=DIRECTION('',(0.,0.,1.));
#5773=DIRECTION('center_axis',(0.,0.,-1.));
#5774=DIRECTION('ref_axis',(1.,0.,0.));
#5775=DIRECTION('center_axis',(0.,0.,1.));
#5776=DIRECTION('ref_axis',(1.,0.,0.));
#5777=DIRECTION('center_axis',(0.,0.,1.));
#5778=DIRECTION('ref_axis',(1.,0.,0.));
#5779=DIRECTION('',(0.,0.,1.));
#5780=DIRECTION('center_axis',(0.,0.,-1.));
#5781=DIRECTION('ref_axis',(1.,0.,0.));
#5782=DIRECTION('center_axis',(0.,1.,0.));
#5783=DIRECTION('ref_axis',(-1.,0.,0.));
#5784=DIRECTION('',(-1.,0.,0.));
#5785=DIRECTION('',(0.,0.,1.));
#5786=DIRECTION('',(-1.,0.,0.));
#5787=DIRECTION('',(0.,0.,1.));
#5788=DIRECTION('center_axis',(1.,0.,0.));
#5789=DIRECTION('ref_axis',(0.,1.,0.));
#5790=DIRECTION('',(0.,1.,0.));
#5791=DIRECTION('',(0.,1.,0.));
#5792=DIRECTION('',(0.,0.,1.));
#5793=DIRECTION('center_axis',(0.,-1.,0.));
#5794=DIRECTION('ref_axis',(1.,0.,0.));
#5795=DIRECTION('',(1.,0.,0.));
#5796=DIRECTION('',(1.,0.,0.));
#5797=DIRECTION('',(0.,0.,1.));
#5798=DIRECTION('center_axis',(-1.,0.,0.));
#5799=DIRECTION('ref_axis',(0.,-1.,0.));
#5800=DIRECTION('',(0.,-1.,0.));
#5801=DIRECTION('',(0.,-1.,0.));
#5802=DIRECTION('center_axis',(0.,0.,1.));
#5803=DIRECTION('ref_axis',(1.,0.,0.));
#5804=DIRECTION('center_axis',(0.,0.,1.));
#5805=DIRECTION('ref_axis',(1.,0.,0.));
#5806=DIRECTION('axis',(0.,0.,1.));
#5807=DIRECTION('refdir',(1.,0.,0.));
#5808=DIRECTION('center_axis',(0.,0.,1.));
#5809=DIRECTION('ref_axis',(1.,0.,0.));
#5810=DIRECTION('center_axis',(0.,0.,-1.));
#5811=DIRECTION('ref_axis',(1.,0.,0.));
#5812=DIRECTION('',(0.,0.,-1.));
#5813=DIRECTION('center_axis',(0.,0.,-1.));
#5814=DIRECTION('ref_axis',(1.,0.,0.));
#5815=DIRECTION('center_axis',(0.,0.,1.));
#5816=DIRECTION('ref_axis',(1.,0.,0.));
#5817=DIRECTION('center_axis',(0.,0.,1.));
#5818=DIRECTION('ref_axis',(1.,0.,0.));
#5819=DIRECTION('',(0.,0.,-1.));
#5820=DIRECTION('center_axis',(0.,0.,1.));
#5821=DIRECTION('ref_axis',(1.,0.,0.));
#5822=DIRECTION('center_axis',(0.,0.,1.));
#5823=DIRECTION('ref_axis',(1.,0.,0.));
#5824=DIRECTION('center_axis',(0.,0.,1.));
#5825=DIRECTION('ref_axis',(1.,0.,0.));
#5826=DIRECTION('axis',(0.,0.,1.));
#5827=DIRECTION('refdir',(1.,0.,0.));
#5828=DIRECTION('center_axis',(0.,0.,1.));
#5829=DIRECTION('ref_axis',(1.,0.,0.));
#5830=DIRECTION('center_axis',(0.,0.,-1.));
#5831=DIRECTION('ref_axis',(1.,0.,0.));
#5832=DIRECTION('',(0.,0.,-1.));
#5833=DIRECTION('center_axis',(0.,0.,-1.));
#5834=DIRECTION('ref_axis',(1.,0.,0.));
#5835=DIRECTION('center_axis',(0.,0.,1.));
#5836=DIRECTION('ref_axis',(1.,0.,0.));
#5837=DIRECTION('center_axis',(0.,0.,1.));
#5838=DIRECTION('ref_axis',(1.,0.,0.));
#5839=DIRECTION('',(0.,0.,-1.));
#5840=DIRECTION('center_axis',(0.,0.,1.));
#5841=DIRECTION('ref_axis',(1.,0.,0.));
#5842=DIRECTION('center_axis',(0.,0.,1.));
#5843=DIRECTION('ref_axis',(1.,0.,0.));
#5844=DIRECTION('center_axis',(0.,0.,1.));
#5845=DIRECTION('ref_axis',(1.,0.,0.));
#5846=DIRECTION('axis',(0.,0.,1.));
#5847=DIRECTION('refdir',(1.,0.,0.));
#5848=DIRECTION('center_axis',(0.,0.,1.));
#5849=DIRECTION('ref_axis',(1.,0.,0.));
#5850=DIRECTION('center_axis',(0.,0.,1.));
#5851=DIRECTION('ref_axis',(1.,0.,0.));
#5852=DIRECTION('',(0.,0.,1.));
#5853=DIRECTION('center_axis',(0.,0.,-1.));
#5854=DIRECTION('ref_axis',(1.,0.,0.));
#5855=DIRECTION('center_axis',(0.,0.,1.));
#5856=DIRECTION('ref_axis',(1.,0.,0.));
#5857=DIRECTION('center_axis',(0.,0.,1.));
#5858=DIRECTION('ref_axis',(1.,0.,0.));
#5859=DIRECTION('',(0.,0.,1.));
#5860=DIRECTION('center_axis',(0.,0.,-1.));
#5861=DIRECTION('ref_axis',(1.,0.,0.));
#5862=DIRECTION('center_axis',(0.,0.,1.));
#5863=DIRECTION('ref_axis',(1.,0.,0.));
#5864=DIRECTION('center_axis',(0.,0.,1.));
#5865=DIRECTION('ref_axis',(1.,0.,0.));
#5866=DIRECTION('',(0.,0.,1.));
#5867=DIRECTION('center_axis',(0.,0.,-1.));
#5868=DIRECTION('ref_axis',(1.,0.,0.));
#5869=DIRECTION('center_axis',(0.,0.,1.));
#5870=DIRECTION('ref_axis',(1.,0.,0.));
#5871=DIRECTION('center_axis',(0.,0.,1.));
#5872=DIRECTION('ref_axis',(1.,0.,0.));
#5873=DIRECTION('',(0.,0.,1.));
#5874=DIRECTION('center_axis',(0.,0.,-1.));
#5875=DIRECTION('ref_axis',(1.,0.,0.));
#5876=DIRECTION('center_axis',(0.,1.,0.));
#5877=DIRECTION('ref_axis',(-1.,0.,0.));
#5878=DIRECTION('',(-1.,0.,0.));
#5879=DIRECTION('',(0.,0.,1.));
#5880=DIRECTION('',(-1.,0.,0.));
#5881=DIRECTION('',(0.,0.,1.));
#5882=DIRECTION('center_axis',(1.,0.,0.));
#5883=DIRECTION('ref_axis',(0.,1.,0.));
#5884=DIRECTION('',(0.,1.,0.));
#5885=DIRECTION('',(0.,1.,0.));
#5886=DIRECTION('',(0.,0.,1.));
#5887=DIRECTION('center_axis',(0.,-1.,0.));
#5888=DIRECTION('ref_axis',(1.,0.,0.));
#5889=DIRECTION('',(1.,0.,0.));
#5890=DIRECTION('',(1.,0.,0.));
#5891=DIRECTION('',(0.,0.,1.));
#5892=DIRECTION('center_axis',(-1.,0.,0.));
#5893=DIRECTION('ref_axis',(0.,-1.,0.));
#5894=DIRECTION('',(0.,-1.,0.));
#5895=DIRECTION('',(0.,-1.,0.));
#5896=DIRECTION('center_axis',(0.,0.,1.));
#5897=DIRECTION('ref_axis',(1.,0.,0.));
#5898=DIRECTION('center_axis',(0.,0.,1.));
#5899=DIRECTION('ref_axis',(1.,0.,0.));
#5900=DIRECTION('axis',(0.,0.,1.));
#5901=DIRECTION('refdir',(1.,0.,0.));
#5902=DIRECTION('center_axis',(0.,0.,1.));
#5903=DIRECTION('ref_axis',(1.,0.,0.));
#5904=DIRECTION('center_axis',(0.,0.,-1.));
#5905=DIRECTION('ref_axis',(1.,0.,0.));
#5906=DIRECTION('',(0.,0.,-1.));
#5907=DIRECTION('center_axis',(0.,0.,-1.));
#5908=DIRECTION('ref_axis',(1.,0.,0.));
#5909=DIRECTION('center_axis',(0.,0.,1.));
#5910=DIRECTION('ref_axis',(1.,0.,0.));
#5911=DIRECTION('center_axis',(0.,0.,1.));
#5912=DIRECTION('ref_axis',(1.,0.,0.));
#5913=DIRECTION('',(0.,0.,-1.));
#5914=DIRECTION('center_axis',(0.,0.,1.));
#5915=DIRECTION('ref_axis',(1.,0.,0.));
#5916=DIRECTION('center_axis',(0.,0.,1.));
#5917=DIRECTION('ref_axis',(1.,0.,0.));
#5918=DIRECTION('center_axis',(0.,0.,1.));
#5919=DIRECTION('ref_axis',(1.,0.,0.));
#5920=DIRECTION('axis',(0.,0.,1.));
#5921=DIRECTION('refdir',(1.,0.,0.));
#5922=DIRECTION('center_axis',(0.,0.,1.));
#5923=DIRECTION('ref_axis',(1.,0.,0.));
#5924=DIRECTION('center_axis',(0.,0.,-1.));
#5925=DIRECTION('ref_axis',(1.,0.,0.));
#5926=DIRECTION('',(0.,0.,-1.));
#5927=DIRECTION('center_axis',(0.,0.,-1.));
#5928=DIRECTION('ref_axis',(1.,0.,0.));
#5929=DIRECTION('center_axis',(0.,0.,1.));
#5930=DIRECTION('ref_axis',(1.,0.,0.));
#5931=DIRECTION('center_axis',(0.,0.,1.));
#5932=DIRECTION('ref_axis',(1.,0.,0.));
#5933=DIRECTION('',(0.,0.,-1.));
#5934=DIRECTION('center_axis',(0.,0.,1.));
#5935=DIRECTION('ref_axis',(1.,0.,0.));
#5936=DIRECTION('center_axis',(0.,0.,1.));
#5937=DIRECTION('ref_axis',(1.,0.,0.));
#5938=DIRECTION('center_axis',(0.,0.,1.));
#5939=DIRECTION('ref_axis',(1.,0.,0.));
#5940=DIRECTION('axis',(0.,0.,1.));
#5941=DIRECTION('refdir',(1.,0.,0.));
#5942=DIRECTION('axis',(0.,0.,1.));
#5943=DIRECTION('refdir',(1.,0.,0.));
#5944=DIRECTION('center_axis',(0.,1.,0.));
#5945=DIRECTION('ref_axis',(1.,0.,0.));
#5946=DIRECTION('center_axis',(0.,1.,0.));
#5947=DIRECTION('ref_axis',(1.,0.,0.));
#5948=DIRECTION('',(0.,1.,0.));
#5949=DIRECTION('center_axis',(0.,-1.,0.));
#5950=DIRECTION('ref_axis',(1.,0.,0.));
#5951=DIRECTION('center_axis',(0.,1.,0.));
#5952=DIRECTION('ref_axis',(1.,0.,0.));
#5953=DIRECTION('center_axis',(0.,1.,0.));
#5954=DIRECTION('ref_axis',(1.,0.,0.));
#5955=DIRECTION('',(0.,1.,0.));
#5956=DIRECTION('center_axis',(0.,-1.,0.));
#5957=DIRECTION('ref_axis',(1.,0.,0.));
#5958=DIRECTION('center_axis',(6.12323399573677E-17,0.,1.));
#5959=DIRECTION('ref_axis',(1.,0.,0.));
#5960=DIRECTION('center_axis',(-1.22464679914735E-16,1.,0.));
#5961=DIRECTION('ref_axis',(-1.,-1.22464679914735E-16,0.));
#5962=DIRECTION('center_axis',(0.,1.,0.));
#5963=DIRECTION('ref_axis',(0.,0.,1.));
#5964=DIRECTION('',(1.,0.,0.));
#5965=DIRECTION('',(0.850265146687862,0.,0.526354614616295));
#5966=DIRECTION('center_axis',(0.,1.,0.));
#5967=DIRECTION('ref_axis',(1.,0.,0.));
#5968=DIRECTION('center_axis',(0.,1.,0.));
#5969=DIRECTION('ref_axis',(0.,0.,1.));
#5970=DIRECTION('',(1.,0.,0.));
#5971=DIRECTION('center_axis',(0.,1.,0.));
#5972=DIRECTION('ref_axis',(1.,0.,0.));
#5973=DIRECTION('',(0.850265146687862,0.,-0.526354614616295));
#5974=DIRECTION('center_axis',(0.,-1.,0.));
#5975=DIRECTION('ref_axis',(0.,0.,-1.));
#5976=DIRECTION('',(-1.,0.,0.));
#5977=DIRECTION('center_axis',(0.,-1.,0.));
#5978=DIRECTION('ref_axis',(1.,0.,0.));
#5979=DIRECTION('',(-0.850265146687862,0.,-0.526354614616295));
#5980=DIRECTION('center_axis',(-0.526354614616295,0.,0.850265146687862));
#5981=DIRECTION('ref_axis',(0.850265146687862,0.,0.526354614616295));
#5982=DIRECTION('',(0.,1.,0.));
#5983=DIRECTION('',(0.,-1.,0.));
#5984=DIRECTION('center_axis',(0.,-1.,0.));
#5985=DIRECTION('ref_axis',(0.,0.,-1.));
#5986=DIRECTION('',(-1.,0.,0.));
#5987=DIRECTION('',(-0.850265146687862,0.,0.526354614616295));
#5988=DIRECTION('center_axis',(0.,-1.,0.));
#5989=DIRECTION('ref_axis',(1.,0.,0.));
#5990=DIRECTION('center_axis',(0.526354614616295,0.,0.850265146687862));
#5991=DIRECTION('ref_axis',(0.850265146687862,0.,-0.526354614616295));
#5992=DIRECTION('',(0.,-1.,0.));
#5993=DIRECTION('',(0.,1.,0.));
#5994=DIRECTION('center_axis',(0.,0.,1.));
#5995=DIRECTION('ref_axis',(1.,0.,0.));
#5996=DIRECTION('',(0.,-1.,0.));
#5997=DIRECTION('',(1.,0.,0.));
#5998=DIRECTION('',(0.,1.,0.));
#5999=DIRECTION('',(-1.,0.,0.));
#6000=DIRECTION('center_axis',(0.,0.,-1.));
#6001=DIRECTION('ref_axis',(1.,0.,0.));
#6002=DIRECTION('center_axis',(0.,0.,-1.));
#6003=DIRECTION('ref_axis',(1.,0.,0.));
#6004=DIRECTION('',(0.,-1.,0.));
#6005=DIRECTION('',(-1.,0.,0.));
#6006=DIRECTION('',(0.,1.,0.));
#6007=DIRECTION('',(0.,1.,0.));
#6008=DIRECTION('',(1.,0.,0.));
#6009=DIRECTION('',(0.,-1.,0.));
#6010=DIRECTION('center_axis',(0.,1.,0.));
#6011=DIRECTION('ref_axis',(6.12323399573677E-17,0.,1.));
#6012=DIRECTION('center_axis',(0.,1.,0.));
#6013=DIRECTION('ref_axis',(1.,0.,0.));
#6014=DIRECTION('center_axis',(0.,-1.,0.));
#6015=DIRECTION('ref_axis',(1.,0.,0.));
#6016=DIRECTION('center_axis',(0.,1.,0.));
#6017=DIRECTION('ref_axis',(1.,0.,0.));
#6018=DIRECTION('center_axis',(0.,1.,0.));
#6019=DIRECTION('ref_axis',(1.,0.,0.));
#6020=DIRECTION('center_axis',(0.,1.,0.));
#6021=DIRECTION('ref_axis',(-1.,0.,0.));
#6022=DIRECTION('',(-1.,0.,0.));
#6023=DIRECTION('',(0.,0.,1.));
#6024=DIRECTION('',(-1.,0.,0.));
#6025=DIRECTION('',(0.,0.,1.));
#6026=DIRECTION('center_axis',(1.,0.,0.));
#6027=DIRECTION('ref_axis',(0.,1.,0.));
#6028=DIRECTION('',(0.,1.,0.));
#6029=DIRECTION('',(0.,0.,1.));
#6030=DIRECTION('',(0.,1.,0.));
#6031=DIRECTION('center_axis',(0.,-1.,0.));
#6032=DIRECTION('ref_axis',(1.,0.,0.));
#6033=DIRECTION('',(1.,0.,0.));
#6034=DIRECTION('',(0.,0.,1.));
#6035=DIRECTION('',(1.,0.,0.));
#6036=DIRECTION('center_axis',(-1.,0.,0.));
#6037=DIRECTION('ref_axis',(0.,-1.,0.));
#6038=DIRECTION('',(0.,-1.,0.));
#6039=DIRECTION('',(0.,-1.,0.));
#6040=DIRECTION('center_axis',(0.,0.,1.));
#6041=DIRECTION('ref_axis',(1.,0.,0.));
#6042=DIRECTION('center_axis',(0.,0.,1.));
#6043=DIRECTION('ref_axis',(1.,0.,0.));
#6044=DIRECTION('center_axis',(0.,0.,1.));
#6045=DIRECTION('ref_axis',(1.,0.,0.));
#6046=DIRECTION('',(0.,0.,1.));
#6047=DIRECTION('center_axis',(0.,0.,1.));
#6048=DIRECTION('ref_axis',(1.,0.,0.));
#6049=DIRECTION('center_axis',(0.,0.,1.));
#6050=DIRECTION('ref_axis',(1.,0.,0.));
#6051=DIRECTION('',(0.,0.,1.));
#6052=DIRECTION('center_axis',(0.,1.,0.));
#6053=DIRECTION('ref_axis',(-1.,0.,0.));
#6054=DIRECTION('',(-1.,0.,0.));
#6055=DIRECTION('',(0.,0.,1.));
#6056=DIRECTION('',(0.,0.,1.));
#6057=DIRECTION('center_axis',(1.,0.,0.));
#6058=DIRECTION('ref_axis',(0.,1.,0.));
#6059=DIRECTION('',(0.,1.,0.));
#6060=DIRECTION('',(0.,0.,1.));
#6061=DIRECTION('center_axis',(0.,-1.,0.));
#6062=DIRECTION('ref_axis',(1.,0.,0.));
#6063=DIRECTION('',(1.,0.,0.));
#6064=DIRECTION('',(0.,0.,1.));
#6065=DIRECTION('center_axis',(-1.,0.,0.));
#6066=DIRECTION('ref_axis',(0.,-1.,0.));
#6067=DIRECTION('',(0.,-1.,0.));
#6068=DIRECTION('center_axis',(0.,0.,1.));
#6069=DIRECTION('ref_axis',(1.,0.,0.));
#6070=DIRECTION('axis',(0.,0.,1.));
#6071=DIRECTION('refdir',(1.,0.,0.));
#6072=DIRECTION('center_axis',(0.,-1.,0.));
#6073=DIRECTION('ref_axis',(1.,0.,0.));
#6074=DIRECTION('center_axis',(0.,-1.,0.));
#6075=DIRECTION('ref_axis',(1.,0.,0.));
#6076=DIRECTION('',(0.,1.,0.));
#6077=DIRECTION('center_axis',(0.,-1.,0.));
#6078=DIRECTION('ref_axis',(1.,0.,0.));
#6079=DIRECTION('center_axis',(0.,1.,0.));
#6080=DIRECTION('ref_axis',(0.,0.,1.));
#6081=DIRECTION('center_axis',(0.,-1.,0.));
#6082=DIRECTION('ref_axis',(1.,0.,0.));
#6083=DIRECTION('center_axis',(6.12323399573677E-17,0.,1.));
#6084=DIRECTION('ref_axis',(1.,0.,0.));
#6085=DIRECTION('center_axis',(1.22464679914735E-16,-1.,0.));
#6086=DIRECTION('ref_axis',(-1.,-1.22464679914735E-16,0.));
#6087=DIRECTION('center_axis',(0.,-1.,0.));
#6088=DIRECTION('ref_axis',(1.,0.,0.));
#6089=DIRECTION('center_axis',(0.,-1.,0.));
#6090=DIRECTION('ref_axis',(0.,0.,-1.));
#6091=DIRECTION('center_axis',(-0.866025403784438,0.,-0.5));
#6092=DIRECTION('ref_axis',(-0.5,0.,0.866025403784438));
#6093=DIRECTION('',(-0.866025403784438,0.,-0.5));
#6094=DIRECTION('center_axis',(-0.866025403784438,0.,-0.5));
#6095=DIRECTION('ref_axis',(-0.5,0.,0.866025403784438));
#6096=DIRECTION('',(-0.866025403784438,0.,-0.5));
#6097=DIRECTION('center_axis',(0.,-1.,0.));
#6098=DIRECTION('ref_axis',(1.,0.,0.));
#6099=DIRECTION('center_axis',(0.,-1.,0.));
#6100=DIRECTION('ref_axis',(1.,0.,0.));
#6101=DIRECTION('',(0.,1.,0.));
#6102=DIRECTION('center_axis',(0.,-1.,0.));
#6103=DIRECTION('ref_axis',(1.,0.,0.));
#6104=DIRECTION('center_axis',(0.866025403784439,0.,-0.5));
#6105=DIRECTION('ref_axis',(-0.5,0.,-0.866025403784439));
#6106=DIRECTION('',(0.866025403784439,0.,-0.5));
#6107=DIRECTION('center_axis',(0.866025403784439,0.,-0.5));
#6108=DIRECTION('ref_axis',(-0.5,0.,-0.866025403784439));
#6109=DIRECTION('',(0.866025403784439,0.,-0.5));
#6110=DIRECTION('center_axis',(0.,0.,1.));
#6111=DIRECTION('ref_axis',(1.,0.,0.));
#6112=DIRECTION('',(0.,0.,1.));
#6113=DIRECTION('center_axis',(0.,0.,1.));
#6114=DIRECTION('ref_axis',(1.,0.,0.));
#6115=DIRECTION('',(0.,0.,1.));
#6116=DIRECTION('center_axis',(0.,1.,0.));
#6117=DIRECTION('ref_axis',(0.,0.,1.));
#6118=DIRECTION('center_axis',(0.,-1.,0.));
#6119=DIRECTION('ref_axis',(1.,0.,0.));
#6120=DIRECTION('center_axis',(0.,1.,0.));
#6121=DIRECTION('ref_axis',(0.,0.,1.));
#6122=DIRECTION('center_axis',(0.,-1.,0.));
#6123=DIRECTION('ref_axis',(1.,0.,0.));
#6124=DIRECTION('center_axis',(0.,-1.,0.));
#6125=DIRECTION('ref_axis',(1.,0.,0.));
#6126=DIRECTION('center_axis',(0.,-1.,0.));
#6127=DIRECTION('ref_axis',(1.,0.,0.));
#6128=DIRECTION('',(0.,1.,0.));
#6129=DIRECTION('center_axis',(0.,-1.,0.));
#6130=DIRECTION('ref_axis',(0.,0.,-1.));
#6131=DIRECTION('center_axis',(0.,-1.,0.));
#6132=DIRECTION('ref_axis',(1.,0.,0.));
#6133=DIRECTION('center_axis',(0.,-1.,0.));
#6134=DIRECTION('ref_axis',(1.,0.,0.));
#6135=DIRECTION('',(0.,1.,0.));
#6136=DIRECTION('',(0.,0.,1.));
#6137=DIRECTION('',(1.,0.,0.));
#6138=DIRECTION('',(0.,0.,1.));
#6139=DIRECTION('',(1.,0.,0.));
#6140=DIRECTION('axis',(0.,0.,1.));
#6141=DIRECTION('refdir',(1.,0.,0.));
#6142=DIRECTION('center_axis',(0.,1.,0.));
#6143=DIRECTION('ref_axis',(1.,0.,0.));
#6144=DIRECTION('center_axis',(0.,-1.,0.));
#6145=DIRECTION('ref_axis',(1.,0.,0.));
#6146=DIRECTION('',(0.,-1.,0.));
#6147=DIRECTION('center_axis',(0.,-1.,0.));
#6148=DIRECTION('ref_axis',(1.,0.,0.));
#6149=DIRECTION('center_axis',(0.,1.,0.));
#6150=DIRECTION('ref_axis',(1.,0.,0.));
#6151=DIRECTION('center_axis',(0.,1.,0.));
#6152=DIRECTION('ref_axis',(1.,0.,0.));
#6153=DIRECTION('',(0.,-1.,0.));
#6154=DIRECTION('center_axis',(0.,1.,0.));
#6155=DIRECTION('ref_axis',(1.,0.,0.));
#6156=DIRECTION('center_axis',(0.,1.,0.));
#6157=DIRECTION('ref_axis',(1.,0.,0.));
#6158=DIRECTION('center_axis',(0.,1.,0.));
#6159=DIRECTION('ref_axis',(1.,0.,0.));
#6160=DIRECTION('axis',(0.,0.,1.));
#6161=DIRECTION('refdir',(1.,0.,0.));
#6162=DIRECTION('center_axis',(0.866025403784439,0.,-0.5));
#6163=DIRECTION('ref_axis',(0.5,0.,0.866025403784439));
#6164=DIRECTION('',(-0.5,0.,-0.866025403784439));
#6165=DIRECTION('',(0.,-1.,0.));
#6166=DIRECTION('',(0.5,0.,0.866025403784439));
#6167=DIRECTION('',(0.,-1.,0.));
#6168=DIRECTION('center_axis',(1.60246890531964E-16,0.,-1.));
#6169=DIRECTION('ref_axis',(1.,0.,1.60246890531964E-16));
#6170=DIRECTION('',(-1.,0.,-1.60246890531964E-16));
#6171=DIRECTION('',(0.,-1.,0.));
#6172=DIRECTION('',(1.,0.,1.60246890531964E-16));
#6173=DIRECTION('center_axis',(-0.866025403784439,0.,-0.5));
#6174=DIRECTION('ref_axis',(0.5,0.,-0.866025403784439));
#6175=DIRECTION('',(-0.5,0.,0.866025403784439));
#6176=DIRECTION('',(0.,-1.,0.));
#6177=DIRECTION('',(0.5,0.,-0.866025403784439));
#6178=DIRECTION('center_axis',(-0.866025403784439,0.,0.5));
#6179=DIRECTION('ref_axis',(-0.5,0.,-0.866025403784439));
#6180=DIRECTION('',(0.5,0.,0.866025403784439));
#6181=DIRECTION('',(0.,-1.,0.));
#6182=DIRECTION('',(-0.5,0.,-0.866025403784439));
#6183=DIRECTION('center_axis',(-1.60246890531964E-16,0.,1.));
#6184=DIRECTION('ref_axis',(-1.,0.,-1.60246890531964E-16));
#6185=DIRECTION('',(1.,0.,1.60246890531964E-16));
#6186=DIRECTION('',(0.,-1.,0.));
#6187=DIRECTION('',(-1.,0.,-1.60246890531964E-16));
#6188=DIRECTION('center_axis',(0.866025403784439,0.,0.5));
#6189=DIRECTION('ref_axis',(-0.5,0.,0.866025403784439));
#6190=DIRECTION('',(0.5,0.,-0.866025403784439));
#6191=DIRECTION('',(-0.5,0.,0.866025403784439));
#6192=DIRECTION('center_axis',(0.,1.,0.));
#6193=DIRECTION('ref_axis',(1.,0.,0.));
#6194=DIRECTION('center_axis',(0.,-1.,0.));
#6195=DIRECTION('ref_axis',(0.,0.,-1.));
#6196=DIRECTION('center_axis',(0.,1.,0.));
#6197=DIRECTION('ref_axis',(1.,0.,0.));
#6198=DIRECTION('center_axis',(0.,1.,0.));
#6199=DIRECTION('ref_axis',(1.,0.,0.));
#6200=DIRECTION('center_axis',(0.,1.,0.));
#6201=DIRECTION('ref_axis',(0.,0.,1.));
#6202=DIRECTION('center_axis',(0.,-1.,0.));
#6203=DIRECTION('ref_axis',(1.,0.,0.));
#6204=DIRECTION('center_axis',(0.,-1.,0.));
#6205=DIRECTION('ref_axis',(1.,0.,0.));
#6206=DIRECTION('center_axis',(0.,-1.,0.));
#6207=DIRECTION('ref_axis',(1.,0.,0.));
#6208=DIRECTION('',(0.707106781186548,0.707106781186547,8.65956056235493E-17));
#6209=DIRECTION('center_axis',(0.,-1.,0.));
#6210=DIRECTION('ref_axis',(1.,0.,0.));
#6211=DIRECTION('center_axis',(0.,-1.,0.));
#6212=DIRECTION('ref_axis',(1.,0.,0.));
#6213=DIRECTION('',(0.,1.,0.));
#6214=DIRECTION('center_axis',(0.,1.,0.));
#6215=DIRECTION('ref_axis',(1.,0.,0.));
#6216=DIRECTION('center_axis',(0.,-1.,0.));
#6217=DIRECTION('ref_axis',(1.,0.,0.));
#6218=DIRECTION('',(-0.707106781186548,0.707106781186547,-8.65956056235494E-17));
#6219=DIRECTION('center_axis',(0.,-1.,0.));
#6220=DIRECTION('ref_axis',(0.,0.,-1.));
#6221=DIRECTION('center_axis',(0.,-1.,0.));
#6222=DIRECTION('ref_axis',(1.,0.,0.));
#6223=DIRECTION('center_axis',(0.,1.,0.));
#6224=DIRECTION('ref_axis',(1.,0.,0.));
#6225=DIRECTION('center_axis',(0.,1.,0.));
#6226=DIRECTION('ref_axis',(1.,0.,0.));
#6227=DIRECTION('',(-0.447213595499958,0.894427190999916,-5.47678698264203E-17));
#6228=DIRECTION('center_axis',(0.,-1.,0.));
#6229=DIRECTION('ref_axis',(1.,0.,0.));
#6230=DIRECTION('',(0.,1.,0.));
#6231=DIRECTION('axis',(0.,0.,1.));
#6232=DIRECTION('refdir',(1.,0.,0.));
#6233=DIRECTION('axis',(0.,0.,1.));
#6234=DIRECTION('refdir',(1.,0.,0.));
#6235=DIRECTION('center_axis',(0.,1.,0.));
#6236=DIRECTION('ref_axis',(1.,0.,0.));
#6237=DIRECTION('center_axis',(0.,1.,0.));
#6238=DIRECTION('ref_axis',(1.,0.,0.));
#6239=DIRECTION('',(0.,1.,0.));
#6240=DIRECTION('center_axis',(0.,1.,0.));
#6241=DIRECTION('ref_axis',(1.,0.,0.));
#6242=DIRECTION('center_axis',(0.,1.,0.));
#6243=DIRECTION('ref_axis',(1.,0.,0.));
#6244=DIRECTION('center_axis',(-1.,0.,0.));
#6245=DIRECTION('ref_axis',(0.,0.,1.));
#6246=DIRECTION('',(0.,-1.,0.));
#6247=DIRECTION('',(0.,0.,1.));
#6248=DIRECTION('',(0.,1.,0.));
#6249=DIRECTION('',(0.,0.,-1.));
#6250=DIRECTION('center_axis',(0.,1.,0.));
#6251=DIRECTION('ref_axis',(1.,0.,0.));
#6252=DIRECTION('center_axis',(0.,-1.,0.));
#6253=DIRECTION('ref_axis',(1.,0.,0.));
#6254=DIRECTION('',(-1.,0.,0.));
#6255=DIRECTION('',(0.,0.,1.));
#6256=DIRECTION('center_axis',(1.,0.,0.));
#6257=DIRECTION('ref_axis',(0.,0.,-1.));
#6258=DIRECTION('',(0.,1.,0.));
#6259=DIRECTION('',(0.,1.,0.));
#6260=DIRECTION('',(0.,0.,-1.));
#6261=DIRECTION('center_axis',(0.,0.,1.));
#6262=DIRECTION('ref_axis',(1.,0.,0.));
#6263=DIRECTION('',(1.,0.,0.));
#6264=DIRECTION('center_axis',(0.,1.,0.));
#6265=DIRECTION('ref_axis',(0.,0.,1.));
#6266=DIRECTION('center_axis',(0.,1.,0.));
#6267=DIRECTION('ref_axis',(1.,0.,0.));
#6268=DIRECTION('center_axis',(0.,1.,0.));
#6269=DIRECTION('ref_axis',(1.,0.,0.));
#6270=DIRECTION('center_axis',(0.,1.,0.));
#6271=DIRECTION('ref_axis',(1.,0.,0.));
#6272=DIRECTION('',(0.,-1.,0.));
#6273=DIRECTION('center_axis',(0.,1.,0.));
#6274=DIRECTION('ref_axis',(1.,0.,0.));
#6275=DIRECTION('center_axis',(0.,1.,0.));
#6276=DIRECTION('ref_axis',(1.,0.,0.));
#6277=DIRECTION('center_axis',(0.,1.,0.));
#6278=DIRECTION('ref_axis',(1.,0.,0.));
#6279=DIRECTION('axis',(0.,0.,1.));
#6280=DIRECTION('refdir',(1.,0.,0.));
#6281=DIRECTION('center_axis',(0.,1.,0.));
#6282=DIRECTION('ref_axis',(1.,0.,0.));
#6283=DIRECTION('center_axis',(0.,1.,0.));
#6284=DIRECTION('ref_axis',(1.,0.,0.));
#6285=DIRECTION('',(0.,1.,0.));
#6286=DIRECTION('center_axis',(0.,-1.,0.));
#6287=DIRECTION('ref_axis',(1.,0.,0.));
#6288=DIRECTION('center_axis',(0.,1.,0.));
#6289=DIRECTION('ref_axis',(1.,0.,0.));
#6290=DIRECTION('center_axis',(0.,1.,0.));
#6291=DIRECTION('ref_axis',(1.,0.,0.));
#6292=DIRECTION('',(0.,1.,0.));
#6293=DIRECTION('center_axis',(0.,-1.,0.));
#6294=DIRECTION('ref_axis',(1.,0.,0.));
#6295=DIRECTION('center_axis',(0.,1.,0.));
#6296=DIRECTION('ref_axis',(1.,0.,0.));
#6297=DIRECTION('center_axis',(0.,1.,0.));
#6298=DIRECTION('ref_axis',(1.,0.,0.));
#6299=DIRECTION('',(0.,1.,0.));
#6300=DIRECTION('center_axis',(0.,-1.,0.));
#6301=DIRECTION('ref_axis',(1.,0.,0.));
#6302=DIRECTION('center_axis',(0.,1.,0.));
#6303=DIRECTION('ref_axis',(1.,0.,0.));
#6304=DIRECTION('center_axis',(0.,1.,0.));
#6305=DIRECTION('ref_axis',(1.,0.,0.));
#6306=DIRECTION('',(0.,1.,0.));
#6307=DIRECTION('center_axis',(0.,-1.,0.));
#6308=DIRECTION('ref_axis',(1.,0.,0.));
#6309=DIRECTION('center_axis',(0.,0.,1.));
#6310=DIRECTION('ref_axis',(1.,0.,0.));
#6311=DIRECTION('',(0.,1.,0.));
#6312=DIRECTION('center_axis',(0.,0.,1.));
#6313=DIRECTION('ref_axis',(1.,0.,0.));
#6314=DIRECTION('center_axis',(0.,0.,1.));
#6315=DIRECTION('ref_axis',(1.,0.,0.));
#6316=DIRECTION('center_axis',(0.,0.,1.));
#6317=DIRECTION('ref_axis',(1.,0.,0.));
#6318=DIRECTION('',(0.,0.,1.));
#6319=DIRECTION('center_axis',(0.,0.,1.));
#6320=DIRECTION('ref_axis',(1.,0.,0.));
#6321=DIRECTION('center_axis',(0.,0.,1.));
#6322=DIRECTION('ref_axis',(1.,0.,0.));
#6323=DIRECTION('',(0.,-1.,0.));
#6324=DIRECTION('center_axis',(-1.,0.,0.));
#6325=DIRECTION('ref_axis',(0.,0.,1.));
#6326=DIRECTION('',(0.,0.,1.));
#6327=DIRECTION('',(0.,1.,0.));
#6328=DIRECTION('',(0.,0.,-1.));
#6329=DIRECTION('',(0.,1.,0.));
#6330=DIRECTION('center_axis',(0.,0.,-1.));
#6331=DIRECTION('ref_axis',(-1.,0.,0.));
#6332=DIRECTION('',(-1.,0.,0.));
#6333=DIRECTION('',(0.,1.,0.));
#6334=DIRECTION('',(1.,0.,0.));
#6335=DIRECTION('center_axis',(1.,0.,0.));
#6336=DIRECTION('ref_axis',(0.,0.,-1.));
#6337=DIRECTION('',(0.,0.,-1.));
#6338=DIRECTION('',(0.,-1.,0.));
#6339=DIRECTION('',(0.,0.,1.));
#6340=DIRECTION('center_axis',(0.,1.,0.));
#6341=DIRECTION('ref_axis',(1.,0.,0.));
#6342=DIRECTION('center_axis',(0.,1.,0.));
#6343=DIRECTION('ref_axis',(1.,0.,0.));
#6344=DIRECTION('center_axis',(0.,-1.,0.));
#6345=DIRECTION('ref_axis',(1.,0.,0.));
#6346=DIRECTION('center_axis',(0.,1.,0.));
#6347=DIRECTION('ref_axis',(1.,0.,0.));
#6348=DIRECTION('center_axis',(0.,1.,0.));
#6349=DIRECTION('ref_axis',(1.,0.,0.));
#6350=DIRECTION('',(0.,1.,0.));
#6351=DIRECTION('center_axis',(0.,-1.,0.));
#6352=DIRECTION('ref_axis',(1.,0.,0.));
#6353=DIRECTION('center_axis',(0.,1.,0.));
#6354=DIRECTION('ref_axis',(1.,0.,0.));
#6355=DIRECTION('center_axis',(0.,1.,0.));
#6356=DIRECTION('ref_axis',(1.,0.,0.));
#6357=DIRECTION('center_axis',(0.,1.,0.));
#6358=DIRECTION('ref_axis',(1.,0.,0.));
#6359=DIRECTION('center_axis',(0.,1.,0.));
#6360=DIRECTION('ref_axis',(1.,0.,0.));
#6361=DIRECTION('center_axis',(0.,-1.,0.));
#6362=DIRECTION('ref_axis',(1.,0.,0.));
#6363=DIRECTION('center_axis',(0.,1.,0.));
#6364=DIRECTION('ref_axis',(1.,0.,0.));
#6365=DIRECTION('center_axis',(0.,1.,0.));
#6366=DIRECTION('ref_axis',(1.,0.,0.));
#6367=DIRECTION('',(0.,-1.,0.));
#6368=DIRECTION('center_axis',(0.,1.,0.));
#6369=DIRECTION('ref_axis',(6.12323399573677E-17,0.,1.));
#6370=DIRECTION('center_axis',(0.,1.,0.));
#6371=DIRECTION('ref_axis',(1.,0.,0.));
#6372=DIRECTION('',(0.,-1.,0.));
#6373=DIRECTION('center_axis',(0.,1.,0.));
#6374=DIRECTION('ref_axis',(1.,0.,0.));
#6375=DIRECTION('axis',(0.,0.,1.));
#6376=DIRECTION('refdir',(1.,0.,0.));
#6377=DIRECTION('center_axis',(0.,1.,0.));
#6378=DIRECTION('ref_axis',(1.,0.,0.));
#6379=DIRECTION('center_axis',(0.,-1.,0.));
#6380=DIRECTION('ref_axis',(1.,0.,0.));
#6381=DIRECTION('',(0.,-1.,0.));
#6382=DIRECTION('center_axis',(0.,-1.,0.));
#6383=DIRECTION('ref_axis',(1.,0.,0.));
#6384=DIRECTION('center_axis',(0.,1.,0.));
#6385=DIRECTION('ref_axis',(1.,0.,0.));
#6386=DIRECTION('center_axis',(0.,1.,0.));
#6387=DIRECTION('ref_axis',(1.,0.,0.));
#6388=DIRECTION('',(0.,-1.,0.));
#6389=DIRECTION('center_axis',(0.,1.,0.));
#6390=DIRECTION('ref_axis',(1.,0.,0.));
#6391=DIRECTION('center_axis',(0.,1.,0.));
#6392=DIRECTION('ref_axis',(1.,0.,0.));
#6393=DIRECTION('center_axis',(0.,1.,0.));
#6394=DIRECTION('ref_axis',(1.,0.,0.));
#6395=DIRECTION('axis',(0.,0.,1.));
#6396=DIRECTION('refdir',(1.,0.,0.));
#6397=DIRECTION('center_axis',(0.,1.,0.));
#6398=DIRECTION('ref_axis',(1.,0.,0.));
#6399=DIRECTION('center_axis',(0.,1.,0.));
#6400=DIRECTION('ref_axis',(1.,0.,0.));
#6401=DIRECTION('',(0.,1.,0.));
#6402=DIRECTION('center_axis',(0.,-1.,0.));
#6403=DIRECTION('ref_axis',(1.,0.,0.));
#6404=DIRECTION('center_axis',(0.,1.,0.));
#6405=DIRECTION('ref_axis',(1.,0.,0.));
#6406=DIRECTION('center_axis',(-1.,0.,0.));
#6407=DIRECTION('ref_axis',(0.,0.,1.));
#6408=DIRECTION('',(0.,-1.,0.));
#6409=DIRECTION('',(0.,0.,1.));
#6410=DIRECTION('',(0.,1.,0.));
#6411=DIRECTION('',(0.,0.,-1.));
#6412=DIRECTION('center_axis',(0.,1.,0.));
#6413=DIRECTION('ref_axis',(1.,0.,0.));
#6414=DIRECTION('center_axis',(0.,-1.,0.));
#6415=DIRECTION('ref_axis',(1.,0.,0.));
#6416=DIRECTION('',(-1.,0.,0.));
#6417=DIRECTION('',(0.,0.,1.));
#6418=DIRECTION('center_axis',(1.,0.,0.));
#6419=DIRECTION('ref_axis',(0.,0.,-1.));
#6420=DIRECTION('',(0.,1.,0.));
#6421=DIRECTION('',(0.,1.,0.));
#6422=DIRECTION('',(0.,0.,-1.));
#6423=DIRECTION('center_axis',(0.,0.,1.));
#6424=DIRECTION('ref_axis',(1.,0.,0.));
#6425=DIRECTION('',(1.,0.,0.));
#6426=DIRECTION('center_axis',(0.,1.,0.));
#6427=DIRECTION('ref_axis',(0.,0.,1.));
#6428=DIRECTION('center_axis',(0.,1.,0.));
#6429=DIRECTION('ref_axis',(1.,0.,0.));
#6430=DIRECTION('center_axis',(0.,1.,0.));
#6431=DIRECTION('ref_axis',(1.,0.,0.));
#6432=DIRECTION('center_axis',(0.,1.,0.));
#6433=DIRECTION('ref_axis',(1.,0.,0.));
#6434=DIRECTION('',(0.,-1.,0.));
#6435=DIRECTION('center_axis',(0.,1.,0.));
#6436=DIRECTION('ref_axis',(1.,0.,0.));
#6437=DIRECTION('center_axis',(0.,1.,0.));
#6438=DIRECTION('ref_axis',(1.,0.,0.));
#6439=DIRECTION('center_axis',(0.,1.,0.));
#6440=DIRECTION('ref_axis',(1.,0.,0.));
#6441=DIRECTION('axis',(0.,0.,1.));
#6442=DIRECTION('refdir',(1.,0.,0.));
#6443=DIRECTION('center_axis',(0.,1.,0.));
#6444=DIRECTION('ref_axis',(1.,0.,0.));
#6445=DIRECTION('center_axis',(0.,1.,0.));
#6446=DIRECTION('ref_axis',(1.,0.,0.));
#6447=DIRECTION('',(0.,1.,0.));
#6448=DIRECTION('center_axis',(0.,-1.,0.));
#6449=DIRECTION('ref_axis',(1.,0.,0.));
#6450=DIRECTION('center_axis',(0.,1.,0.));
#6451=DIRECTION('ref_axis',(1.,0.,0.));
#6452=DIRECTION('center_axis',(0.,1.,0.));
#6453=DIRECTION('ref_axis',(1.,0.,0.));
#6454=DIRECTION('',(0.,1.,0.));
#6455=DIRECTION('center_axis',(0.,-1.,0.));
#6456=DIRECTION('ref_axis',(1.,0.,0.));
#6457=DIRECTION('center_axis',(0.,1.,0.));
#6458=DIRECTION('ref_axis',(1.,0.,0.));
#6459=DIRECTION('center_axis',(0.,1.,0.));
#6460=DIRECTION('ref_axis',(1.,0.,0.));
#6461=DIRECTION('',(0.,1.,0.));
#6462=DIRECTION('center_axis',(0.,-1.,0.));
#6463=DIRECTION('ref_axis',(1.,0.,0.));
#6464=DIRECTION('center_axis',(0.,1.,0.));
#6465=DIRECTION('ref_axis',(1.,0.,0.));
#6466=DIRECTION('center_axis',(0.,1.,0.));
#6467=DIRECTION('ref_axis',(1.,0.,0.));
#6468=DIRECTION('',(0.,1.,0.));
#6469=DIRECTION('center_axis',(0.,-1.,0.));
#6470=DIRECTION('ref_axis',(1.,0.,0.));
#6471=DIRECTION('center_axis',(0.,0.,1.));
#6472=DIRECTION('ref_axis',(1.,0.,0.));
#6473=DIRECTION('',(0.,1.,0.));
#6474=DIRECTION('center_axis',(0.,0.,1.));
#6475=DIRECTION('ref_axis',(1.,0.,0.));
#6476=DIRECTION('center_axis',(0.,0.,1.));
#6477=DIRECTION('ref_axis',(1.,0.,0.));
#6478=DIRECTION('center_axis',(0.,0.,1.));
#6479=DIRECTION('ref_axis',(1.,0.,0.));
#6480=DIRECTION('',(0.,0.,1.));
#6481=DIRECTION('center_axis',(0.,0.,1.));
#6482=DIRECTION('ref_axis',(1.,0.,0.));
#6483=DIRECTION('center_axis',(0.,0.,1.));
#6484=DIRECTION('ref_axis',(1.,0.,0.));
#6485=DIRECTION('',(0.,-1.,0.));
#6486=DIRECTION('center_axis',(1.,0.,0.));
#6487=DIRECTION('ref_axis',(0.,0.,-1.));
#6488=DIRECTION('',(0.,0.,1.));
#6489=DIRECTION('',(0.,1.,0.));
#6490=DIRECTION('',(0.,0.,-1.));
#6491=DIRECTION('',(0.,-1.,0.));
#6492=DIRECTION('center_axis',(-1.,0.,0.));
#6493=DIRECTION('ref_axis',(0.,0.,1.));
#6494=DIRECTION('',(0.,0.,-1.));
#6495=DIRECTION('',(0.,1.,0.));
#6496=DIRECTION('',(0.,0.,1.));
#6497=DIRECTION('',(0.,1.,0.));
#6498=DIRECTION('center_axis',(0.,0.,-1.));
#6499=DIRECTION('ref_axis',(-1.,0.,0.));
#6500=DIRECTION('',(1.,0.,0.));
#6501=DIRECTION('',(-1.,0.,0.));
#6502=DIRECTION('center_axis',(0.,1.,0.));
#6503=DIRECTION('ref_axis',(1.,0.,0.));
#6504=DIRECTION('center_axis',(0.,1.,0.));
#6505=DIRECTION('ref_axis',(1.,0.,0.));
#6506=DIRECTION('center_axis',(0.,-1.,0.));
#6507=DIRECTION('ref_axis',(1.,0.,0.));
#6508=DIRECTION('center_axis',(0.,1.,0.));
#6509=DIRECTION('ref_axis',(6.12323399573677E-17,0.,1.));
#6510=DIRECTION('center_axis',(0.,-1.,0.));
#6511=DIRECTION('ref_axis',(1.,0.,0.));
#6512=DIRECTION('center_axis',(0.,1.,0.));
#6513=DIRECTION('ref_axis',(1.,0.,0.));
#6514=DIRECTION('center_axis',(0.,1.,0.));
#6515=DIRECTION('ref_axis',(1.,0.,0.));
#6516=DIRECTION('',(0.,1.,0.));
#6517=DIRECTION('center_axis',(0.,1.,0.));
#6518=DIRECTION('ref_axis',(1.,0.,0.));
#6519=DIRECTION('center_axis',(0.,1.,0.));
#6520=DIRECTION('ref_axis',(1.,0.,0.));
#6521=DIRECTION('center_axis',(0.,1.,0.));
#6522=DIRECTION('ref_axis',(1.,0.,0.));
#6523=DIRECTION('center_axis',(0.,1.,0.));
#6524=DIRECTION('ref_axis',(1.,0.,0.));
#6525=DIRECTION('',(0.,-1.,0.));
#6526=DIRECTION('center_axis',(0.,1.,0.));
#6527=DIRECTION('ref_axis',(1.,0.,0.));
#6528=DIRECTION('center_axis',(0.,1.,0.));
#6529=DIRECTION('ref_axis',(1.,0.,0.));
#6530=DIRECTION('center_axis',(0.,1.,0.));
#6531=DIRECTION('ref_axis',(1.,0.,0.));
#6532=DIRECTION('',(0.,-1.,0.));
#6533=DIRECTION('center_axis',(0.,1.,0.));
#6534=DIRECTION('ref_axis',(1.,0.,0.));
#6535=DIRECTION('center_axis',(0.,1.,0.));
#6536=DIRECTION('ref_axis',(1.,0.,0.));
#6537=DIRECTION('axis',(0.,0.,1.));
#6538=DIRECTION('refdir',(1.,0.,0.));
#6539=DIRECTION('center_axis',(0.,1.,0.));
#6540=DIRECTION('ref_axis',(1.,0.,0.));
#6541=DIRECTION('center_axis',(0.,-1.,0.));
#6542=DIRECTION('ref_axis',(1.,0.,0.));
#6543=DIRECTION('',(0.,-1.,0.));
#6544=DIRECTION('center_axis',(0.,-1.,0.));
#6545=DIRECTION('ref_axis',(1.,0.,0.));
#6546=DIRECTION('center_axis',(0.,1.,0.));
#6547=DIRECTION('ref_axis',(1.,0.,0.));
#6548=DIRECTION('center_axis',(0.,1.,0.));
#6549=DIRECTION('ref_axis',(1.,0.,0.));
#6550=DIRECTION('',(0.,-1.,0.));
#6551=DIRECTION('center_axis',(0.,1.,0.));
#6552=DIRECTION('ref_axis',(1.,0.,0.));
#6553=DIRECTION('center_axis',(0.,1.,0.));
#6554=DIRECTION('ref_axis',(1.,0.,0.));
#6555=DIRECTION('center_axis',(0.,1.,0.));
#6556=DIRECTION('ref_axis',(1.,0.,0.));
#6557=DIRECTION('axis',(0.,0.,1.));
#6558=DIRECTION('refdir',(1.,0.,0.));
#6559=DIRECTION('center_axis',(0.,1.,0.));
#6560=DIRECTION('ref_axis',(1.,0.,0.));
#6561=DIRECTION('center_axis',(0.,-1.,0.));
#6562=DIRECTION('ref_axis',(1.,0.,0.));
#6563=DIRECTION('',(0.,-1.,0.));
#6564=DIRECTION('center_axis',(0.,-1.,0.));
#6565=DIRECTION('ref_axis',(1.,0.,0.));
#6566=DIRECTION('center_axis',(0.,1.,0.));
#6567=DIRECTION('ref_axis',(1.,0.,0.));
#6568=DIRECTION('center_axis',(0.,1.,0.));
#6569=DIRECTION('ref_axis',(1.,0.,0.));
#6570=DIRECTION('',(0.,-1.,0.));
#6571=DIRECTION('center_axis',(0.,1.,0.));
#6572=DIRECTION('ref_axis',(1.,0.,0.));
#6573=DIRECTION('center_axis',(0.,1.,0.));
#6574=DIRECTION('ref_axis',(1.,0.,0.));
#6575=DIRECTION('center_axis',(0.,1.,0.));
#6576=DIRECTION('ref_axis',(1.,0.,0.));
#6577=DIRECTION('axis',(0.,0.,1.));
#6578=DIRECTION('refdir',(1.,0.,0.));
#6579=DIRECTION('center_axis',(0.,0.,1.));
#6580=DIRECTION('ref_axis',(1.,0.,0.));
#6581=DIRECTION('',(0.,1.,0.));
#6582=DIRECTION('center_axis',(0.,0.,1.));
#6583=DIRECTION('ref_axis',(1.,0.,0.));
#6584=DIRECTION('center_axis',(0.,0.,1.));
#6585=DIRECTION('ref_axis',(1.,0.,0.));
#6586=DIRECTION('center_axis',(0.,0.,1.));
#6587=DIRECTION('ref_axis',(1.,0.,0.));
#6588=DIRECTION('',(0.,0.,1.));
#6589=DIRECTION('center_axis',(0.,0.,1.));
#6590=DIRECTION('ref_axis',(1.,0.,0.));
#6591=DIRECTION('center_axis',(0.,0.,1.));
#6592=DIRECTION('ref_axis',(1.,0.,0.));
#6593=DIRECTION('',(0.,-1.,0.));
#6594=DIRECTION('center_axis',(0.,1.,0.));
#6595=DIRECTION('ref_axis',(1.,0.,0.));
#6596=DIRECTION('center_axis',(0.,-1.,0.));
#6597=DIRECTION('ref_axis',(1.,0.,0.));
#6598=DIRECTION('',(0.,-1.,0.));
#6599=DIRECTION('center_axis',(0.,-1.,0.));
#6600=DIRECTION('ref_axis',(1.,0.,0.));
#6601=DIRECTION('center_axis',(0.,1.,0.));
#6602=DIRECTION('ref_axis',(1.,0.,0.));
#6603=DIRECTION('center_axis',(0.,1.,0.));
#6604=DIRECTION('ref_axis',(1.,0.,0.));
#6605=DIRECTION('',(0.,-1.,0.));
#6606=DIRECTION('center_axis',(0.,1.,0.));
#6607=DIRECTION('ref_axis',(1.,0.,0.));
#6608=DIRECTION('center_axis',(0.,1.,0.));
#6609=DIRECTION('ref_axis',(1.,0.,0.));
#6610=DIRECTION('center_axis',(0.,1.,0.));
#6611=DIRECTION('ref_axis',(1.,0.,0.));
#6612=DIRECTION('axis',(0.,0.,1.));
#6613=DIRECTION('refdir',(1.,0.,0.));
#6614=DIRECTION('center_axis',(0.,0.,1.));
#6615=DIRECTION('ref_axis',(1.,0.,0.));
#6616=DIRECTION('',(0.,1.,0.));
#6617=DIRECTION('center_axis',(0.,0.,1.));
#6618=DIRECTION('ref_axis',(1.,0.,0.));
#6619=DIRECTION('center_axis',(0.,0.,1.));
#6620=DIRECTION('ref_axis',(1.,0.,0.));
#6621=DIRECTION('center_axis',(0.,0.,1.));
#6622=DIRECTION('ref_axis',(1.,0.,0.));
#6623=DIRECTION('',(0.,0.,1.));
#6624=DIRECTION('center_axis',(0.,0.,1.));
#6625=DIRECTION('ref_axis',(1.,0.,0.));
#6626=DIRECTION('center_axis',(0.,0.,1.));
#6627=DIRECTION('ref_axis',(1.,0.,0.));
#6628=DIRECTION('',(0.,-1.,0.));
#6629=DIRECTION('center_axis',(0.,1.,0.));
#6630=DIRECTION('ref_axis',(1.,0.,0.));
#6631=DIRECTION('center_axis',(0.,-1.,0.));
#6632=DIRECTION('ref_axis',(1.,0.,0.));
#6633=DIRECTION('',(0.,-1.,0.));
#6634=DIRECTION('center_axis',(0.,-1.,0.));
#6635=DIRECTION('ref_axis',(1.,0.,0.));
#6636=DIRECTION('center_axis',(0.,1.,0.));
#6637=DIRECTION('ref_axis',(1.,0.,0.));
#6638=DIRECTION('center_axis',(0.,1.,0.));
#6639=DIRECTION('ref_axis',(1.,0.,0.));
#6640=DIRECTION('',(0.,-1.,0.));
#6641=DIRECTION('center_axis',(0.,1.,0.));
#6642=DIRECTION('ref_axis',(1.,0.,0.));
#6643=DIRECTION('center_axis',(0.,1.,0.));
#6644=DIRECTION('ref_axis',(1.,0.,0.));
#6645=DIRECTION('center_axis',(0.,1.,0.));
#6646=DIRECTION('ref_axis',(1.,0.,0.));
#6647=DIRECTION('axis',(0.,0.,1.));
#6648=DIRECTION('refdir',(1.,0.,0.));
#6649=DIRECTION('center_axis',(1.,0.,0.));
#6650=DIRECTION('ref_axis',(0.,0.,-1.));
#6651=DIRECTION('',(0.,-0.707106781186547,-0.707106781186548));
#6652=DIRECTION('',(0.,-1.,0.));
#6653=DIRECTION('',(0.,-0.707106781186547,0.707106781186548));
#6654=DIRECTION('',(0.,0.,1.));
#6655=DIRECTION('',(0.,0.707106781186547,0.707106781186548));
#6656=DIRECTION('',(0.,1.,0.));
#6657=DIRECTION('',(0.,0.707106781186547,-0.707106781186548));
#6658=DIRECTION('',(0.,0.,-1.));
#6659=DIRECTION('center_axis',(0.,0.707106781186548,-0.707106781186547));
#6660=DIRECTION('ref_axis',(-1.,0.,0.));
#6661=DIRECTION('',(1.,0.,0.));
#6662=DIRECTION('',(0.,-0.707106781186547,-0.707106781186548));
#6663=DIRECTION('',(-1.,0.,0.));
#6664=DIRECTION('center_axis',(0.,1.,0.));
#6665=DIRECTION('ref_axis',(-1.,0.,0.));
#6666=DIRECTION('',(-1.,0.,0.));
#6667=DIRECTION('',(0.,0.,-1.));
#6668=DIRECTION('center_axis',(0.,0.707106781186548,0.707106781186547));
#6669=DIRECTION('ref_axis',(1.,0.,0.));
#6670=DIRECTION('',(1.,0.,0.));
#6671=DIRECTION('',(0.,0.707106781186547,-0.707106781186548));
#6672=DIRECTION('center_axis',(0.,0.,1.));
#6673=DIRECTION('ref_axis',(1.,0.,0.));
#6674=DIRECTION('',(-1.,0.,0.));
#6675=DIRECTION('',(0.,1.,0.));
#6676=DIRECTION('center_axis',(1.,0.,0.));
#6677=DIRECTION('ref_axis',(0.,0.,-1.));
#6678=DIRECTION('',(0.,-0.707106781186547,0.707106781186548));
#6679=DIRECTION('',(0.,-1.,0.));
#6680=DIRECTION('',(0.,0.707106781186547,0.707106781186548));
#6681=DIRECTION('',(0.,0.,1.));
#6682=DIRECTION('center_axis',(0.,0.,1.));
#6683=DIRECTION('ref_axis',(1.,0.,0.));
#6684=DIRECTION('',(1.,0.,0.));
#6685=DIRECTION('center_axis',(0.,-0.707106781186548,0.707106781186547));
#6686=DIRECTION('ref_axis',(1.,0.,0.));
#6687=DIRECTION('',(1.,0.,0.));
#6688=DIRECTION('center_axis',(0.,-0.707106781186548,-0.707106781186547));
#6689=DIRECTION('ref_axis',(-1.,0.,0.));
#6690=DIRECTION('',(-1.,0.,0.));
#6691=DIRECTION('center_axis',(0.,-1.,0.));
#6692=DIRECTION('ref_axis',(1.,0.,0.));
#6693=DIRECTION('axis',(0.,0.,1.));
#6694=DIRECTION('refdir',(1.,0.,0.));
#6695=DIRECTION('center_axis',(0.,1.,0.));
#6696=DIRECTION('ref_axis',(0.,0.,1.));
#6697=DIRECTION('center_axis',(0.,-1.,0.));
#6698=DIRECTION('ref_axis',(1.,0.,0.));
#6699=DIRECTION('center_axis',(0.,-1.,0.));
#6700=DIRECTION('ref_axis',(1.,0.,0.));
#6701=DIRECTION('center_axis',(0.,-1.,0.));
#6702=DIRECTION('ref_axis',(1.,0.,0.));
#6703=DIRECTION('',(0.707106781186548,0.707106781186547,8.65956056235493E-17));
#6704=DIRECTION('center_axis',(0.,-1.,0.));
#6705=DIRECTION('ref_axis',(1.,0.,0.));
#6706=DIRECTION('center_axis',(0.,-1.,0.));
#6707=DIRECTION('ref_axis',(1.,0.,0.));
#6708=DIRECTION('',(0.,1.,0.));
#6709=DIRECTION('center_axis',(0.,1.,0.));
#6710=DIRECTION('ref_axis',(1.,0.,0.));
#6711=DIRECTION('center_axis',(0.,-1.,0.));
#6712=DIRECTION('ref_axis',(1.,0.,0.));
#6713=DIRECTION('',(-0.707106781186547,0.707106781186548,-8.65956056235493E-17));
#6714=DIRECTION('center_axis',(0.,-1.,0.));
#6715=DIRECTION('ref_axis',(0.,0.,-1.));
#6716=DIRECTION('center_axis',(0.,-1.,0.));
#6717=DIRECTION('ref_axis',(1.,0.,0.));
#6718=DIRECTION('center_axis',(0.,1.,0.));
#6719=DIRECTION('ref_axis',(1.,0.,0.));
#6720=DIRECTION('center_axis',(0.,1.,0.));
#6721=DIRECTION('ref_axis',(1.,0.,0.));
#6722=DIRECTION('',(-0.447213595499958,0.894427190999916,-5.47678698264203E-17));
#6723=DIRECTION('center_axis',(0.,-1.,0.));
#6724=DIRECTION('ref_axis',(1.,0.,0.));
#6725=DIRECTION('center_axis',(0.,1.,0.));
#6726=DIRECTION('ref_axis',(1.,0.,0.));
#6727=DIRECTION('',(0.,1.,0.));
#6728=DIRECTION('center_axis',(0.,1.,0.));
#6729=DIRECTION('ref_axis',(1.,0.,0.));
#6730=DIRECTION('center_axis',(0.,-1.,0.));
#6731=DIRECTION('ref_axis',(1.,0.,0.));
#6732=DIRECTION('',(-0.707106781186547,0.707106781186548,-8.65956056235493E-17));
#6733=DIRECTION('center_axis',(0.,-1.,0.));
#6734=DIRECTION('ref_axis',(0.,0.,-1.));
#6735=DIRECTION('center_axis',(0.866025403784439,0.,-0.5));
#6736=DIRECTION('ref_axis',(0.5,0.,0.866025403784439));
#6737=DIRECTION('',(-0.5,0.,-0.866025403784439));
#6738=DIRECTION('',(0.,-1.,0.));
#6739=DIRECTION('',(0.5,0.,0.866025403784439));
#6740=DIRECTION('',(0.,-1.,0.));
#6741=DIRECTION('center_axis',(1.20185167898973E-16,0.,-1.));
#6742=DIRECTION('ref_axis',(1.,0.,1.20185167898973E-16));
#6743=DIRECTION('',(-1.,0.,-1.20185167898973E-16));
#6744=DIRECTION('',(0.,-1.,0.));
#6745=DIRECTION('',(1.,0.,1.20185167898973E-16));
#6746=DIRECTION('center_axis',(-0.866025403784439,0.,-0.5));
#6747=DIRECTION('ref_axis',(0.5,0.,-0.866025403784439));
#6748=DIRECTION('',(-0.5,0.,0.866025403784439));
#6749=DIRECTION('',(0.,-1.,0.));
#6750=DIRECTION('',(0.5,0.,-0.866025403784439));
#6751=DIRECTION('center_axis',(-0.866025403784439,0.,0.5));
#6752=DIRECTION('ref_axis',(-0.5,0.,-0.866025403784439));
#6753=DIRECTION('',(0.5,0.,0.866025403784439));
#6754=DIRECTION('',(0.,-1.,0.));
#6755=DIRECTION('',(-0.5,0.,-0.866025403784439));
#6756=DIRECTION('center_axis',(-2.40370335797945E-16,0.,1.));
#6757=DIRECTION('ref_axis',(-1.,0.,-2.40370335797945E-16));
#6758=DIRECTION('',(1.,0.,2.40370335797945E-16));
#6759=DIRECTION('',(0.,-1.,0.));
#6760=DIRECTION('',(-1.,0.,-2.40370335797945E-16));
#6761=DIRECTION('center_axis',(0.866025403784439,0.,0.5));
#6762=DIRECTION('ref_axis',(-0.5,0.,0.866025403784439));
#6763=DIRECTION('',(0.5,0.,-0.866025403784439));
#6764=DIRECTION('',(-0.5,0.,0.866025403784439));
#6765=DIRECTION('center_axis',(0.,1.,0.));
#6766=DIRECTION('ref_axis',(1.,0.,0.));
#6767=DIRECTION('center_axis',(0.,-1.,0.));
#6768=DIRECTION('ref_axis',(0.,0.,-1.));
#6769=DIRECTION('axis',(0.,0.,1.));
#6770=DIRECTION('refdir',(1.,0.,0.));
#6771=DIRECTION('center_axis',(0.,1.,0.));
#6772=DIRECTION('ref_axis',(0.,0.,1.));
#6773=DIRECTION('center_axis',(0.,-1.,0.));
#6774=DIRECTION('ref_axis',(1.,0.,0.));
#6775=DIRECTION('center_axis',(0.,-1.,0.));
#6776=DIRECTION('ref_axis',(1.,0.,0.));
#6777=DIRECTION('center_axis',(0.,-1.,0.));
#6778=DIRECTION('ref_axis',(1.,0.,0.));
#6779=DIRECTION('',(0.707106781186548,0.707106781186547,8.65956056235494E-17));
#6780=DIRECTION('center_axis',(0.,-1.,0.));
#6781=DIRECTION('ref_axis',(1.,0.,0.));
#6782=DIRECTION('center_axis',(0.,-1.,0.));
#6783=DIRECTION('ref_axis',(1.,0.,0.));
#6784=DIRECTION('',(0.,1.,0.));
#6785=DIRECTION('center_axis',(0.,1.,0.));
#6786=DIRECTION('ref_axis',(1.,0.,0.));
#6787=DIRECTION('center_axis',(0.,-1.,0.));
#6788=DIRECTION('ref_axis',(1.,0.,0.));
#6789=DIRECTION('',(-0.707106781186547,0.707106781186548,-8.65956056235493E-17));
#6790=DIRECTION('center_axis',(0.,-1.,0.));
#6791=DIRECTION('ref_axis',(0.,0.,-1.));
#6792=DIRECTION('center_axis',(0.,-1.,0.));
#6793=DIRECTION('ref_axis',(1.,0.,0.));
#6794=DIRECTION('center_axis',(0.,1.,0.));
#6795=DIRECTION('ref_axis',(1.,0.,0.));
#6796=DIRECTION('center_axis',(0.,1.,0.));
#6797=DIRECTION('ref_axis',(1.,0.,0.));
#6798=DIRECTION('',(-0.447213595499958,0.894427190999916,-5.47678698264203E-17));
#6799=DIRECTION('center_axis',(0.,-1.,0.));
#6800=DIRECTION('ref_axis',(1.,0.,0.));
#6801=DIRECTION('center_axis',(0.,1.,0.));
#6802=DIRECTION('ref_axis',(1.,0.,0.));
#6803=DIRECTION('',(0.,1.,0.));
#6804=DIRECTION('center_axis',(0.,1.,0.));
#6805=DIRECTION('ref_axis',(1.,0.,0.));
#6806=DIRECTION('center_axis',(0.,-1.,0.));
#6807=DIRECTION('ref_axis',(1.,0.,0.));
#6808=DIRECTION('',(-0.707106781186547,0.707106781186548,-8.65956056235493E-17));
#6809=DIRECTION('center_axis',(0.,-1.,0.));
#6810=DIRECTION('ref_axis',(0.,0.,-1.));
#6811=DIRECTION('center_axis',(0.866025403784439,0.,-0.5));
#6812=DIRECTION('ref_axis',(0.5,0.,0.866025403784439));
#6813=DIRECTION('',(-0.5,0.,-0.866025403784439));
#6814=DIRECTION('',(0.,-1.,0.));
#6815=DIRECTION('',(0.5,0.,0.866025403784439));
#6816=DIRECTION('',(0.,-1.,0.));
#6817=DIRECTION('center_axis',(1.92296268638356E-16,0.,-1.));
#6818=DIRECTION('ref_axis',(1.,0.,1.92296268638356E-16));
#6819=DIRECTION('',(-1.,0.,-1.92296268638356E-16));
#6820=DIRECTION('',(0.,-1.,0.));
#6821=DIRECTION('',(1.,0.,1.92296268638356E-16));
#6822=DIRECTION('center_axis',(-0.866025403784439,0.,-0.5));
#6823=DIRECTION('ref_axis',(0.5,0.,-0.866025403784439));
#6824=DIRECTION('',(-0.5,0.,0.866025403784438));
#6825=DIRECTION('',(0.,-1.,0.));
#6826=DIRECTION('',(0.5,0.,-0.866025403784438));
#6827=DIRECTION('center_axis',(-0.866025403784439,0.,0.5));
#6828=DIRECTION('ref_axis',(-0.5,0.,-0.866025403784439));
#6829=DIRECTION('',(0.5,0.,0.866025403784439));
#6830=DIRECTION('',(0.,-1.,0.));
#6831=DIRECTION('',(-0.5,0.,-0.866025403784439));
#6832=DIRECTION('center_axis',(-1.92296268638356E-16,0.,1.));
#6833=DIRECTION('ref_axis',(-1.,0.,-1.92296268638356E-16));
#6834=DIRECTION('',(1.,0.,1.92296268638356E-16));
#6835=DIRECTION('',(0.,-1.,0.));
#6836=DIRECTION('',(-1.,0.,-1.92296268638356E-16));
#6837=DIRECTION('center_axis',(0.866025403784439,0.,0.5));
#6838=DIRECTION('ref_axis',(-0.5,0.,0.866025403784439));
#6839=DIRECTION('',(0.5,0.,-0.866025403784439));
#6840=DIRECTION('',(-0.5,0.,0.866025403784439));
#6841=DIRECTION('center_axis',(0.,1.,0.));
#6842=DIRECTION('ref_axis',(1.,0.,0.));
#6843=DIRECTION('center_axis',(0.,-1.,0.));
#6844=DIRECTION('ref_axis',(0.,0.,-1.));
#6845=DIRECTION('axis',(0.,0.,1.));
#6846=DIRECTION('refdir',(1.,0.,0.));
#6847=DIRECTION('center_axis',(0.,1.,0.));
#6848=DIRECTION('ref_axis',(1.,0.,0.));
#6849=DIRECTION('center_axis',(0.,-1.,0.));
#6850=DIRECTION('ref_axis',(1.,0.,0.));
#6851=DIRECTION('',(0.,-1.,0.));
#6852=DIRECTION('center_axis',(0.,-1.,0.));
#6853=DIRECTION('ref_axis',(1.,0.,0.));
#6854=DIRECTION('center_axis',(0.,1.,0.));
#6855=DIRECTION('ref_axis',(1.,0.,0.));
#6856=DIRECTION('center_axis',(0.,1.,0.));
#6857=DIRECTION('ref_axis',(1.,0.,0.));
#6858=DIRECTION('',(0.,-1.,0.));
#6859=DIRECTION('center_axis',(0.,1.,0.));
#6860=DIRECTION('ref_axis',(1.,0.,0.));
#6861=DIRECTION('center_axis',(0.,1.,0.));
#6862=DIRECTION('ref_axis',(1.,0.,0.));
#6863=DIRECTION('center_axis',(0.,1.,0.));
#6864=DIRECTION('ref_axis',(1.,0.,0.));
#6865=DIRECTION('',(0.,0.,1.));
#6866=DIRECTION('',(1.,0.,0.));
#6867=DIRECTION('',(0.,0.,1.));
#6868=DIRECTION('',(1.,0.,0.));
#6869=DIRECTION('',(0.,0.,1.));
#6870=DIRECTION('',(1.,0.,0.));
#6871=DIRECTION('',(0.,0.,1.));
#6872=DIRECTION('',(1.,0.,0.));
#6873=DIRECTION('',(0.,0.,1.));
#6874=DIRECTION('',(1.,0.,0.));
#6875=DIRECTION('',(0.,0.,1.));
#6876=DIRECTION('',(1.,0.,0.));
#6877=DIRECTION('',(0.,0.,1.));
#6878=DIRECTION('',(1.,0.,0.));
#6879=DIRECTION('',(0.,0.,1.));
#6880=DIRECTION('',(1.,0.,0.));
#6881=DIRECTION('',(0.,0.,1.));
#6882=DIRECTION('',(1.,0.,0.));
#6883=DIRECTION('',(0.,-1.,2.22044604925031E-16));
#6884=DIRECTION('',(1.,0.,0.));
#6885=DIRECTION('',(0.,-1.,2.22044604925031E-16));
#6886=DIRECTION('',(1.,0.,0.));
#6887=DIRECTION('',(0.,-1.,2.22044604925031E-16));
#6888=DIRECTION('',(1.,0.,0.));
#6889=DIRECTION('',(0.,-1.,2.22044604925031E-16));
#6890=DIRECTION('',(1.,0.,0.));
#6891=DIRECTION('',(0.,0.,1.));
#6892=DIRECTION('',(1.,0.,0.));
#6893=DIRECTION('',(0.,-1.,2.22044604925031E-16));
#6894=DIRECTION('',(1.,0.,0.));
#6895=DIRECTION('',(0.,-1.,2.22044604925031E-16));
#6896=DIRECTION('',(1.,0.,0.));
#6897=DIRECTION('',(0.,-1.,2.22044604925031E-16));
#6898=DIRECTION('',(1.,0.,0.));
#6899=DIRECTION('',(0.,-1.,2.22044604925031E-16));
#6900=DIRECTION('',(1.,0.,0.));
#6901=DIRECTION('',(0.,-1.,2.22044604925031E-16));
#6902=DIRECTION('',(1.,0.,0.));
#6903=DIRECTION('',(0.,-1.,2.22044604925031E-16));
#6904=DIRECTION('',(1.,0.,0.));
#6905=DIRECTION('',(0.,-1.,2.22044604925031E-16));
#6906=DIRECTION('',(1.,0.,0.));
#6907=DIRECTION('',(0.,-1.,2.22044604925031E-16));
#6908=DIRECTION('',(1.,0.,0.));
#6909=DIRECTION('',(0.,0.,1.));
#6910=DIRECTION('',(1.,0.,0.));
#6911=DIRECTION('',(0.,-1.,2.22044604925031E-16));
#6912=DIRECTION('',(1.,0.,0.));
#6913=DIRECTION('',(0.,-1.,2.22044604925031E-16));
#6914=DIRECTION('',(1.,0.,0.));
#6915=DIRECTION('',(0.,-1.,2.22044604925031E-16));
#6916=DIRECTION('',(1.,0.,0.));
#6917=DIRECTION('',(0.,-1.,2.22044604925031E-16));
#6918=DIRECTION('',(1.,0.,0.));
#6919=DIRECTION('axis',(0.,0.,1.));
#6920=DIRECTION('refdir',(1.,0.,0.));
#6921=DIRECTION('center_axis',(0.,1.,0.));
#6922=DIRECTION('ref_axis',(1.,0.,0.));
#6923=DIRECTION('',(0.866025403784439,-0.5,1.06057523872491E-16));
#6924=DIRECTION('center_axis',(0.,-1.,0.));
#6925=DIRECTION('ref_axis',(1.,0.,0.));
#6926=DIRECTION('center_axis',(0.,-1.,0.));
#6927=DIRECTION('ref_axis',(1.,0.,0.));
#6928=DIRECTION('center_axis',(0.,1.,0.));
#6929=DIRECTION('ref_axis',(1.,0.,0.));
#6930=DIRECTION('',(-0.866025403784439,-0.5,-1.06057523872491E-16));
#6931=DIRECTION('center_axis',(1.92296268638356E-16,0.,-1.));
#6932=DIRECTION('ref_axis',(-1.,0.,-1.92296268638356E-16));
#6933=DIRECTION('',(0.,1.,0.));
#6934=DIRECTION('',(0.,1.,0.));
#6935=DIRECTION('center_axis',(-0.866025403784439,0.,-0.5));
#6936=DIRECTION('ref_axis',(-0.5,0.,0.866025403784439));
#6937=DIRECTION('',(0.,1.,0.));
#6938=DIRECTION('center_axis',(-0.866025403784439,0.,0.5));
#6939=DIRECTION('ref_axis',(0.5,0.,0.866025403784439));
#6940=DIRECTION('',(0.,1.,0.));
#6941=DIRECTION('center_axis',(0.,1.,0.));
#6942=DIRECTION('ref_axis',(1.,0.,0.));
#6943=DIRECTION('center_axis',(0.,1.,0.));
#6944=DIRECTION('ref_axis',(1.,0.,0.));
#6945=DIRECTION('',(0.,-1.,0.));
#6946=DIRECTION('center_axis',(0.,1.,0.));
#6947=DIRECTION('ref_axis',(1.,0.,0.));
#6948=DIRECTION('center_axis',(-1.92296268638356E-16,0.,1.));
#6949=DIRECTION('ref_axis',(1.,0.,1.92296268638356E-16));
#6950=DIRECTION('',(0.,1.,0.));
#6951=DIRECTION('center_axis',(0.866025403784439,0.,-0.5));
#6952=DIRECTION('ref_axis',(-0.5,0.,-0.866025403784439));
#6953=DIRECTION('',(0.,1.,0.));
#6954=DIRECTION('center_axis',(0.866025403784439,0.,0.5));
#6955=DIRECTION('ref_axis',(0.5,0.,-0.866025403784439));
#6956=DIRECTION('center_axis',(0.,1.,0.));
#6957=DIRECTION('ref_axis',(1.,0.,0.));
#6958=DIRECTION('center_axis',(0.,1.,0.));
#6959=DIRECTION('ref_axis',(1.,0.,0.));
#6960=DIRECTION('axis',(0.,0.,1.));
#6961=DIRECTION('refdir',(1.,0.,0.));
#6962=DIRECTION('center_axis',(0.866025403784439,0.,-0.5));
#6963=DIRECTION('ref_axis',(0.5,0.,0.866025403784439));
#6964=DIRECTION('',(0.5,0.,0.866025403784439));
#6965=DIRECTION('',(0.,-1.,0.));
#6966=DIRECTION('',(0.5,0.,0.866025403784439));
#6967=DIRECTION('',(0.,-1.,0.));
#6968=DIRECTION('center_axis',(1.92296268638356E-16,0.,-1.));
#6969=DIRECTION('ref_axis',(1.,0.,1.92296268638356E-16));
#6970=DIRECTION('',(1.,0.,1.92296268638356E-16));
#6971=DIRECTION('',(0.,-1.,0.));
#6972=DIRECTION('',(1.,0.,1.92296268638356E-16));
#6973=DIRECTION('center_axis',(-0.866025403784439,0.,-0.5));
#6974=DIRECTION('ref_axis',(0.5,0.,-0.866025403784439));
#6975=DIRECTION('',(0.5,0.,-0.866025403784439));
#6976=DIRECTION('',(0.,-1.,0.));
#6977=DIRECTION('',(0.5,0.,-0.866025403784438));
#6978=DIRECTION('center_axis',(-0.866025403784439,0.,0.5));
#6979=DIRECTION('ref_axis',(-0.5,0.,-0.866025403784439));
#6980=DIRECTION('',(-0.5,0.,-0.866025403784439));
#6981=DIRECTION('',(0.,-1.,0.));
#6982=DIRECTION('',(-0.5,0.,-0.866025403784439));
#6983=DIRECTION('center_axis',(-1.92296268638356E-16,0.,1.));
#6984=DIRECTION('ref_axis',(-1.,0.,-1.92296268638356E-16));
#6985=DIRECTION('',(-1.,0.,-1.92296268638356E-16));
#6986=DIRECTION('',(0.,-1.,0.));
#6987=DIRECTION('',(-1.,0.,-1.92296268638356E-16));
#6988=DIRECTION('center_axis',(0.866025403784439,0.,0.5));
#6989=DIRECTION('ref_axis',(-0.5,0.,0.866025403784439));
#6990=DIRECTION('',(-0.5,0.,0.866025403784439));
#6991=DIRECTION('',(-0.5,0.,0.866025403784439));
#6992=DIRECTION('center_axis',(0.,-1.,0.));
#6993=DIRECTION('ref_axis',(0.,0.,-1.));
#6994=DIRECTION('center_axis',(0.,1.,0.));
#6995=DIRECTION('ref_axis',(0.,0.,1.));
#6996=DIRECTION('center_axis',(0.,-1.,0.));
#6997=DIRECTION('ref_axis',(1.,0.,0.));
#6998=DIRECTION('center_axis',(0.,-1.,0.));
#6999=DIRECTION('ref_axis',(1.,0.,0.));
#7000=DIRECTION('center_axis',(0.,-1.,0.));
#7001=DIRECTION('ref_axis',(1.,0.,0.));
#7002=DIRECTION('',(0.707106781186547,0.707106781186548,8.65956056235493E-17));
#7003=DIRECTION('center_axis',(0.,-1.,0.));
#7004=DIRECTION('ref_axis',(1.,0.,0.));
#7005=DIRECTION('center_axis',(0.,1.,0.));
#7006=DIRECTION('ref_axis',(1.,0.,0.));
#7007=DIRECTION('',(0.,1.,0.));
#7008=DIRECTION('center_axis',(0.,1.,0.));
#7009=DIRECTION('ref_axis',(1.,0.,0.));
#7010=DIRECTION('center_axis',(0.,-1.,0.));
#7011=DIRECTION('ref_axis',(1.,0.,0.));
#7012=DIRECTION('',(-0.707106781186547,0.707106781186548,-8.65956056235493E-17));
#7013=DIRECTION('center_axis',(0.,-1.,0.));
#7014=DIRECTION('ref_axis',(0.,0.,-1.));
#7015=DIRECTION('',(0.,0.,1.));
#7016=DIRECTION('',(1.,0.,0.));
#7017=DIRECTION('',(0.,0.,1.));
#7018=DIRECTION('',(1.,0.,0.));
#7019=DIRECTION('',(0.,0.,1.));
#7020=DIRECTION('',(1.,0.,0.));
#7021=DIRECTION('',(0.,0.,1.));
#7022=DIRECTION('',(1.,0.,0.));
#7023=DIRECTION('',(0.,0.,1.));
#7024=DIRECTION('',(1.,0.,0.));
#7025=DIRECTION('',(0.,0.,1.));
#7026=DIRECTION('',(1.,0.,0.));
#7027=DIRECTION('',(0.,0.,1.));
#7028=DIRECTION('',(1.,0.,0.));
#7029=DIRECTION('',(0.,0.,1.));
#7030=DIRECTION('',(1.,0.,0.));
#7031=DIRECTION('',(0.,0.,1.));
#7032=DIRECTION('',(1.,0.,0.));
#7033=DIRECTION('',(8.65956056235493E-17,-8.65956056235493E-17,-1.));
#7034=DIRECTION('',(2.22044604925031E-16,1.,-8.65956056235494E-17));
#7035=DIRECTION('',(0.,-1.,2.22044604925031E-16));
#7036=DIRECTION('',(1.,0.,0.));
#7037=DIRECTION('',(0.,0.,1.));
#7038=DIRECTION('',(-1.,1.22464679914735E-16,0.));
#7039=DIRECTION('',(8.65956056235493E-17,-8.65956056235493E-17,-1.));
#7040=DIRECTION('',(2.22044604925031E-16,1.,-8.65956056235494E-17));
#7041=DIRECTION('',(0.,-1.,2.22044604925031E-16));
#7042=DIRECTION('',(1.,0.,0.));
#7043=DIRECTION('',(0.,0.,1.));
#7044=DIRECTION('',(1.,0.,0.));
#7045=DIRECTION('',(0.,0.,1.));
#7046=DIRECTION('',(1.,0.,0.));
#7047=DIRECTION('',(0.,0.,1.));
#7048=DIRECTION('',(-1.,1.22464679914735E-16,0.));
#7049=DIRECTION('',(0.,0.,1.));
#7050=DIRECTION('',(1.,0.,0.));
#7051=DIRECTION('',(0.,0.,1.));
#7052=DIRECTION('',(1.,0.,0.));
#7053=DIRECTION('',(0.,0.,1.));
#7054=DIRECTION('',(1.,0.,0.));
#7055=DIRECTION('',(0.,0.,1.));
#7056=DIRECTION('',(-1.,1.22464679914735E-16,0.));
#7057=DIRECTION('',(0.,0.,1.));
#7058=DIRECTION('',(1.,0.,0.));
#7059=DIRECTION('',(0.,0.,1.));
#7060=DIRECTION('',(1.,0.,0.));
#7061=DIRECTION('',(0.,0.,1.));
#7062=DIRECTION('',(1.,0.,0.));
#7063=DIRECTION('',(0.,0.,1.));
#7064=DIRECTION('',(-1.,1.22464679914735E-16,0.));
#7065=DIRECTION('',(0.,0.,1.));
#7066=DIRECTION('',(1.,0.,0.));
#7067=DIRECTION('',(0.,0.,1.));
#7068=DIRECTION('',(1.,0.,0.));
#7069=DIRECTION('',(0.,0.,1.));
#7070=DIRECTION('',(1.,0.,0.));
#7071=DIRECTION('',(0.,0.,1.));
#7072=DIRECTION('',(-1.,1.22464679914735E-16,0.));
#7073=DIRECTION('',(0.,0.,1.));
#7074=DIRECTION('',(1.,0.,0.));
#7075=DIRECTION('',(0.,0.,1.));
#7076=DIRECTION('',(1.,0.,0.));
#7077=DIRECTION('',(0.,-1.,2.22044604925031E-16));
#7078=DIRECTION('',(1.,0.,0.));
#7079=DIRECTION('',(0.,-1.,2.22044604925031E-16));
#7080=DIRECTION('',(1.,0.,0.));
#7081=DIRECTION('',(0.,0.,1.));
#7082=DIRECTION('',(1.,0.,0.));
#7083=DIRECTION('',(0.,0.,1.));
#7084=DIRECTION('',(1.,0.,0.));
#7085=CARTESIAN_POINT('',(0.,0.,0.));
#7086=CARTESIAN_POINT('',(0.,0.,0.));
#7087=CARTESIAN_POINT('',(0.,0.,0.));
#7088=CARTESIAN_POINT('Origin',(7.3,0.,-0.1));
#7089=CARTESIAN_POINT('',(7.05,-3.06161699786838E-17,0.));
#7090=CARTESIAN_POINT('Origin',(7.3,0.,0.));
#7091=CARTESIAN_POINT('',(7.05,3.06161699786838E-17,1.2));
#7092=CARTESIAN_POINT('',(7.05,-3.06161699786838E-17,-0.1));
#7093=CARTESIAN_POINT('Origin',(7.3,0.,1.2));
#7094=CARTESIAN_POINT('Origin',(-7.3,20.,-0.1));
#7095=CARTESIAN_POINT('',(-7.55,20.,0.));
#7096=CARTESIAN_POINT('Origin',(-7.3,20.,0.));
#7097=CARTESIAN_POINT('',(-7.55,20.,1.2));
#7098=CARTESIAN_POINT('',(-7.55,20.,-0.1));
#7099=CARTESIAN_POINT('Origin',(-7.3,20.,1.2));
#7100=CARTESIAN_POINT('Origin',(-7.3,0.,-0.1));
#7101=CARTESIAN_POINT('',(-7.55,-3.06161699786838E-17,0.));
#7102=CARTESIAN_POINT('Origin',(-7.3,0.,0.));
#7103=CARTESIAN_POINT('',(-7.55,3.06161699786838E-17,1.2));
#7104=CARTESIAN_POINT('',(-7.55,-3.06161699786838E-17,-0.1));
#7105=CARTESIAN_POINT('Origin',(-7.3,0.,1.2));
#7106=CARTESIAN_POINT('Origin',(7.3,20.,-0.1));
#7107=CARTESIAN_POINT('',(7.05,20.,0.));
#7108=CARTESIAN_POINT('Origin',(7.3,20.,0.));
#7109=CARTESIAN_POINT('',(7.05,20.,1.2));
#7110=CARTESIAN_POINT('',(7.05,20.,-0.1));
#7111=CARTESIAN_POINT('Origin',(7.3,20.,1.2));
#7112=CARTESIAN_POINT('Origin',(9.,24.,0.));
#7113=CARTESIAN_POINT('',(9.,24.,0.));
#7114=CARTESIAN_POINT('',(-9.,24.,0.));
#7115=CARTESIAN_POINT('',(9.,24.,0.));
#7116=CARTESIAN_POINT('',(-9.,24.,1.2));
#7117=CARTESIAN_POINT('',(-9.,24.,0.));
#7118=CARTESIAN_POINT('',(9.,24.,1.2));
#7119=CARTESIAN_POINT('',(9.,24.,1.2));
#7120=CARTESIAN_POINT('',(9.,24.,0.));
#7121=CARTESIAN_POINT('Origin',(9.,-4.,0.));
#7122=CARTESIAN_POINT('',(9.,-4.,0.));
#7123=CARTESIAN_POINT('',(9.,-4.,0.));
#7124=CARTESIAN_POINT('',(9.,-4.,1.2));
#7125=CARTESIAN_POINT('',(9.,-4.,1.2));
#7126=CARTESIAN_POINT('',(9.,-4.,0.));
#7127=CARTESIAN_POINT('Origin',(-9.,-4.,0.));
#7128=CARTESIAN_POINT('',(-9.,-4.,0.));
#7129=CARTESIAN_POINT('',(-9.,-4.,0.));
#7130=CARTESIAN_POINT('',(-9.,-4.,1.2));
#7131=CARTESIAN_POINT('',(-9.,-4.,1.2));
#7132=CARTESIAN_POINT('',(-9.,-4.,0.));
#7133=CARTESIAN_POINT('Origin',(-9.,24.,0.));
#7134=CARTESIAN_POINT('',(-9.,24.,0.));
#7135=CARTESIAN_POINT('',(-9.,24.,1.2));
#7136=CARTESIAN_POINT('Origin',(0.,10.,1.2));
#7137=CARTESIAN_POINT('Origin',(0.,10.,0.));
#7138=CARTESIAN_POINT('',(0.,0.,0.));
#7139=CARTESIAN_POINT('Origin',(9.,-3.,-0.3));
#7140=CARTESIAN_POINT('',(9.,-3.,-0.3));
#7141=CARTESIAN_POINT('',(-9.,-3.,-0.3));
#7142=CARTESIAN_POINT('',(9.,-3.,-0.3));
#7143=CARTESIAN_POINT('',(-9.,-3.,0.));
#7144=CARTESIAN_POINT('',(-9.,-3.,-0.3));
#7145=CARTESIAN_POINT('',(9.,-3.,0.));
#7146=CARTESIAN_POINT('',(9.,-3.,0.));
#7147=CARTESIAN_POINT('',(9.,-3.,-0.3));
#7148=CARTESIAN_POINT('Origin',(9.,-4.,-0.3));
#7149=CARTESIAN_POINT('',(9.,-4.,-0.3));
#7150=CARTESIAN_POINT('',(9.,-4.,-0.3));
#7151=CARTESIAN_POINT('',(9.,-4.,0.));
#7152=CARTESIAN_POINT('',(9.,-4.,0.));
#7153=CARTESIAN_POINT('',(9.,-4.,-0.3));
#7154=CARTESIAN_POINT('Origin',(-9.,-4.,-0.3));
#7155=CARTESIAN_POINT('',(-9.,-4.,-0.3));
#7156=CARTESIAN_POINT('',(-9.,-4.,-0.3));
#7157=CARTESIAN_POINT('',(-9.,-4.,0.));
#7158=CARTESIAN_POINT('',(-9.,-4.,0.));
#7159=CARTESIAN_POINT('',(-9.,-4.,-0.3));
#7160=CARTESIAN_POINT('Origin',(-9.,-3.,-0.3));
#7161=CARTESIAN_POINT('',(-9.,-3.,-0.3));
#7162=CARTESIAN_POINT('',(-9.,-3.,0.));
#7163=CARTESIAN_POINT('Origin',(0.,-3.5,0.));
#7164=CARTESIAN_POINT('Origin',(0.,-3.5,-0.3));
#7165=CARTESIAN_POINT('',(0.,0.,0.));
#7166=CARTESIAN_POINT('Origin',(9.,24.,-0.3));
#7167=CARTESIAN_POINT('',(9.,24.,-0.3));
#7168=CARTESIAN_POINT('',(-9.,24.,-0.3));
#7169=CARTESIAN_POINT('',(9.,24.,-0.3));
#7170=CARTESIAN_POINT('',(-9.,24.,0.));
#7171=CARTESIAN_POINT('',(-9.,24.,-0.3));
#7172=CARTESIAN_POINT('',(9.,24.,0.));
#7173=CARTESIAN_POINT('',(9.,24.,0.));
#7174=CARTESIAN_POINT('',(9.,24.,-0.3));
#7175=CARTESIAN_POINT('Origin',(9.,23.,-0.3));
#7176=CARTESIAN_POINT('',(9.,23.,-0.3));
#7177=CARTESIAN_POINT('',(9.,23.,-0.3));
#7178=CARTESIAN_POINT('',(9.,23.,0.));
#7179=CARTESIAN_POINT('',(9.,23.,0.));
#7180=CARTESIAN_POINT('',(9.,23.,-0.3));
#7181=CARTESIAN_POINT('Origin',(-9.,23.,-0.3));
#7182=CARTESIAN_POINT('',(-9.,23.,-0.3));
#7183=CARTESIAN_POINT('',(-9.,23.,-0.3));
#7184=CARTESIAN_POINT('',(-9.,23.,0.));
#7185=CARTESIAN_POINT('',(-9.,23.,0.));
#7186=CARTESIAN_POINT('',(-9.,23.,-0.3));
#7187=CARTESIAN_POINT('Origin',(-9.,24.,-0.3));
#7188=CARTESIAN_POINT('',(-9.,24.,-0.3));
#7189=CARTESIAN_POINT('',(-9.,24.,0.));
#7190=CARTESIAN_POINT('Origin',(0.,23.5,0.));
#7191=CARTESIAN_POINT('Origin',(0.,23.5,-0.3));
#7192=CARTESIAN_POINT('',(0.,0.,0.));
#7193=CARTESIAN_POINT('Origin',(-4.75,0.,1.1));
#7194=CARTESIAN_POINT('',(-5.09,-4.163799117101E-17,1.2));
#7195=CARTESIAN_POINT('Origin',(-4.75,0.,1.2));
#7196=CARTESIAN_POINT('',(-5.09,4.163799117101E-17,3.2));
#7197=CARTESIAN_POINT('',(-5.09,-4.163799117101E-17,1.1));
#7198=CARTESIAN_POINT('Origin',(-4.75,0.,3.2));
#7199=CARTESIAN_POINT('Origin',(4.75,0.,1.1));
#7200=CARTESIAN_POINT('',(4.41,-4.163799117101E-17,1.2));
#7201=CARTESIAN_POINT('Origin',(4.75,0.,1.2));
#7202=CARTESIAN_POINT('',(4.41,4.163799117101E-17,3.2));
#7203=CARTESIAN_POINT('',(4.41,-4.163799117101E-17,1.1));
#7204=CARTESIAN_POINT('Origin',(4.75,0.,3.2));
#7205=CARTESIAN_POINT('Origin',(-7.3,0.,1.1));
#7206=CARTESIAN_POINT('',(-7.63,-4.04133443718627E-17,1.2));
#7207=CARTESIAN_POINT('Origin',(-7.3,0.,1.2));
#7208=CARTESIAN_POINT('',(-7.63,4.04133443718627E-17,3.2));
#7209=CARTESIAN_POINT('',(-7.63,-4.04133443718627E-17,1.1));
#7210=CARTESIAN_POINT('Origin',(-7.3,0.,3.2));
#7211=CARTESIAN_POINT('Origin',(7.3,0.,1.1));
#7212=CARTESIAN_POINT('',(6.97,-4.04133443718627E-17,1.2));
#7213=CARTESIAN_POINT('Origin',(7.3,0.,1.2));
#7214=CARTESIAN_POINT('',(6.97,4.04133443718627E-17,3.2));
#7215=CARTESIAN_POINT('',(6.97,-4.04133443718627E-17,1.1));
#7216=CARTESIAN_POINT('Origin',(7.3,0.,3.2));
#7217=CARTESIAN_POINT('Origin',(8.,2.5,1.2));
#7218=CARTESIAN_POINT('',(8.,2.5,1.2));
#7219=CARTESIAN_POINT('',(-8.,2.5,1.2));
#7220=CARTESIAN_POINT('',(8.,2.5,1.2));
#7221=CARTESIAN_POINT('',(-8.,2.5,3.2));
#7222=CARTESIAN_POINT('',(-8.,2.5,1.2));
#7223=CARTESIAN_POINT('',(8.,2.5,3.2));
#7224=CARTESIAN_POINT('',(8.,2.5,3.2));
#7225=CARTESIAN_POINT('',(8.,2.5,1.2));
#7226=CARTESIAN_POINT('Origin',(8.,-2.5,1.2));
#7227=CARTESIAN_POINT('',(8.,-2.5,1.2));
#7228=CARTESIAN_POINT('',(8.,-2.5,1.2));
#7229=CARTESIAN_POINT('',(8.,-2.5,3.2));
#7230=CARTESIAN_POINT('',(8.,-2.5,3.2));
#7231=CARTESIAN_POINT('',(8.,-2.5,1.2));
#7232=CARTESIAN_POINT('Origin',(-8.,-2.5,1.2));
#7233=CARTESIAN_POINT('',(-8.,-2.5,1.2));
#7234=CARTESIAN_POINT('',(-8.,-2.5,1.2));
#7235=CARTESIAN_POINT('',(-8.,-2.5,3.2));
#7236=CARTESIAN_POINT('',(-8.,-2.5,3.2));
#7237=CARTESIAN_POINT('',(-8.,-2.5,1.2));
#7238=CARTESIAN_POINT('Origin',(-8.,2.5,1.2));
#7239=CARTESIAN_POINT('',(-8.,2.5,1.2));
#7240=CARTESIAN_POINT('',(-8.,2.5,3.2));
#7241=CARTESIAN_POINT('Origin',(0.,0.,3.2));
#7242=CARTESIAN_POINT('Origin',(0.,0.,1.2));
#7243=CARTESIAN_POINT('',(0.,0.,0.));
#7244=CARTESIAN_POINT('Origin',(-4.75,0.,3.2));
#7245=CARTESIAN_POINT('',(-5.175,-5.20474889637625E-17,4.4));
#7246=CARTESIAN_POINT('Origin',(-4.75,0.,4.4));
#7247=CARTESIAN_POINT('',(-5.175,-5.20474889637625E-17,3.2));
#7248=CARTESIAN_POINT('',(-5.175,-5.20474889637625E-17,3.2));
#7249=CARTESIAN_POINT('Origin',(-4.75,0.,3.2));
#7250=CARTESIAN_POINT('Origin',(-4.75,0.,3.2));
#7251=CARTESIAN_POINT('',(-5.395,-7.89897185450042E-17,4.4));
#7252=CARTESIAN_POINT('Origin',(-4.75,0.,4.4));
#7253=CARTESIAN_POINT('',(-5.395,-7.89897185450042E-17,3.2));
#7254=CARTESIAN_POINT('',(-5.395,-7.89897185450042E-17,3.2));
#7255=CARTESIAN_POINT('Origin',(-4.75,0.,3.2));
#7256=CARTESIAN_POINT('Origin',(-4.75,0.,4.4));
#7257=CARTESIAN_POINT('Origin',(-4.75,0.,3.2));
#7258=CARTESIAN_POINT('',(0.,0.,0.));
#7259=CARTESIAN_POINT('Origin',(4.75,0.,3.2));
#7260=CARTESIAN_POINT('',(4.325,-5.20474889637625E-17,4.4));
#7261=CARTESIAN_POINT('Origin',(4.75,0.,4.4));
#7262=CARTESIAN_POINT('',(4.325,-5.20474889637625E-17,3.2));
#7263=CARTESIAN_POINT('',(4.325,-5.20474889637625E-17,3.2));
#7264=CARTESIAN_POINT('Origin',(4.75,0.,3.2));
#7265=CARTESIAN_POINT('Origin',(4.75,0.,3.2));
#7266=CARTESIAN_POINT('',(4.105,-7.89897185450042E-17,4.4));
#7267=CARTESIAN_POINT('Origin',(4.75,0.,4.4));
#7268=CARTESIAN_POINT('',(4.105,-7.89897185450042E-17,3.2));
#7269=CARTESIAN_POINT('',(4.105,-7.89897185450042E-17,3.2));
#7270=CARTESIAN_POINT('Origin',(4.75,0.,3.2));
#7271=CARTESIAN_POINT('Origin',(4.75,0.,4.4));
#7272=CARTESIAN_POINT('Origin',(4.75,0.,3.2));
#7273=CARTESIAN_POINT('',(0.,0.,0.));
#7274=CARTESIAN_POINT('Origin',(-4.75,20.,1.1));
#7275=CARTESIAN_POINT('',(-5.09,20.,1.2));
#7276=CARTESIAN_POINT('Origin',(-4.75,20.,1.2));
#7277=CARTESIAN_POINT('',(-5.09,20.,3.2));
#7278=CARTESIAN_POINT('',(-5.09,20.,1.1));
#7279=CARTESIAN_POINT('Origin',(-4.75,20.,3.2));
#7280=CARTESIAN_POINT('Origin',(4.75,20.,1.1));
#7281=CARTESIAN_POINT('',(4.41,20.,1.2));
#7282=CARTESIAN_POINT('Origin',(4.75,20.,1.2));
#7283=CARTESIAN_POINT('',(4.41,20.,3.2));
#7284=CARTESIAN_POINT('',(4.41,20.,1.1));
#7285=CARTESIAN_POINT('Origin',(4.75,20.,3.2));
#7286=CARTESIAN_POINT('Origin',(-7.3,20.,1.1));
#7287=CARTESIAN_POINT('',(-7.63,20.,1.2));
#7288=CARTESIAN_POINT('Origin',(-7.3,20.,1.2));
#7289=CARTESIAN_POINT('',(-7.63,20.,3.2));
#7290=CARTESIAN_POINT('',(-7.63,20.,1.1));
#7291=CARTESIAN_POINT('Origin',(-7.3,20.,3.2));
#7292=CARTESIAN_POINT('Origin',(7.3,20.,1.1));
#7293=CARTESIAN_POINT('',(6.97,20.,1.2));
#7294=CARTESIAN_POINT('Origin',(7.3,20.,1.2));
#7295=CARTESIAN_POINT('',(6.97,20.,3.2));
#7296=CARTESIAN_POINT('',(6.97,20.,1.1));
#7297=CARTESIAN_POINT('Origin',(7.3,20.,3.2));
#7298=CARTESIAN_POINT('Origin',(8.,22.5,1.2));
#7299=CARTESIAN_POINT('',(8.,22.5,1.2));
#7300=CARTESIAN_POINT('',(-8.,22.5,1.2));
#7301=CARTESIAN_POINT('',(8.,22.5,1.2));
#7302=CARTESIAN_POINT('',(-8.,22.5,3.2));
#7303=CARTESIAN_POINT('',(-8.,22.5,1.2));
#7304=CARTESIAN_POINT('',(8.,22.5,3.2));
#7305=CARTESIAN_POINT('',(8.,22.5,3.2));
#7306=CARTESIAN_POINT('',(8.,22.5,1.2));
#7307=CARTESIAN_POINT('Origin',(8.,17.5,1.2));
#7308=CARTESIAN_POINT('',(8.,17.5,1.2));
#7309=CARTESIAN_POINT('',(8.,17.5,1.2));
#7310=CARTESIAN_POINT('',(8.,17.5,3.2));
#7311=CARTESIAN_POINT('',(8.,17.5,3.2));
#7312=CARTESIAN_POINT('',(8.,17.5,1.2));
#7313=CARTESIAN_POINT('Origin',(-8.,17.5,1.2));
#7314=CARTESIAN_POINT('',(-8.,17.5,1.2));
#7315=CARTESIAN_POINT('',(-8.,17.5,1.2));
#7316=CARTESIAN_POINT('',(-8.,17.5,3.2));
#7317=CARTESIAN_POINT('',(-8.,17.5,3.2));
#7318=CARTESIAN_POINT('',(-8.,17.5,1.2));
#7319=CARTESIAN_POINT('Origin',(-8.,22.5,1.2));
#7320=CARTESIAN_POINT('',(-8.,22.5,1.2));
#7321=CARTESIAN_POINT('',(-8.,22.5,3.2));
#7322=CARTESIAN_POINT('Origin',(0.,20.,3.2));
#7323=CARTESIAN_POINT('Origin',(0.,20.,1.2));
#7324=CARTESIAN_POINT('',(0.,0.,0.));
#7325=CARTESIAN_POINT('Origin',(-4.75,20.,3.2));
#7326=CARTESIAN_POINT('',(-5.175,20.,4.4));
#7327=CARTESIAN_POINT('Origin',(-4.75,20.,4.4));
#7328=CARTESIAN_POINT('',(-5.175,20.,3.2));
#7329=CARTESIAN_POINT('',(-5.175,20.,3.2));
#7330=CARTESIAN_POINT('Origin',(-4.75,20.,3.2));
#7331=CARTESIAN_POINT('Origin',(-4.75,20.,3.2));
#7332=CARTESIAN_POINT('',(-5.395,20.,4.4));
#7333=CARTESIAN_POINT('Origin',(-4.75,20.,4.4));
#7334=CARTESIAN_POINT('',(-5.395,20.,3.2));
#7335=CARTESIAN_POINT('',(-5.395,20.,3.2));
#7336=CARTESIAN_POINT('Origin',(-4.75,20.,3.2));
#7337=CARTESIAN_POINT('Origin',(-4.75,20.,4.4));
#7338=CARTESIAN_POINT('Origin',(-4.75,20.,3.2));
#7339=CARTESIAN_POINT('',(0.,0.,0.));
#7340=CARTESIAN_POINT('Origin',(4.75,20.,3.2));
#7341=CARTESIAN_POINT('',(4.325,20.,4.4));
#7342=CARTESIAN_POINT('Origin',(4.75,20.,4.4));
#7343=CARTESIAN_POINT('',(4.325,20.,3.2));
#7344=CARTESIAN_POINT('',(4.325,20.,3.2));
#7345=CARTESIAN_POINT('Origin',(4.75,20.,3.2));
#7346=CARTESIAN_POINT('Origin',(4.75,20.,3.2));
#7347=CARTESIAN_POINT('',(4.105,20.,4.4));
#7348=CARTESIAN_POINT('Origin',(4.75,20.,4.4));
#7349=CARTESIAN_POINT('',(4.105,20.,3.2));
#7350=CARTESIAN_POINT('',(4.105,20.,3.2));
#7351=CARTESIAN_POINT('Origin',(4.75,20.,3.2));
#7352=CARTESIAN_POINT('Origin',(4.75,20.,4.4));
#7353=CARTESIAN_POINT('Origin',(4.75,20.,3.2));
#7354=CARTESIAN_POINT('',(0.,0.,0.));
#7355=CARTESIAN_POINT('',(0.,0.,0.));
#7356=CARTESIAN_POINT('Origin',(0.,0.,0.));
#7357=CARTESIAN_POINT('',(-2.05,-1.65,2.51052593825207E-16));
#7358=CARTESIAN_POINT('Origin',(0.,-1.65,0.));
#7359=CARTESIAN_POINT('',(-2.05,-1.14891252930761,-2.51052593825207E-16));
#7360=CARTESIAN_POINT('',(-2.05,0.,2.51052593825207E-16));
#7361=CARTESIAN_POINT('Origin',(0.,-1.14891252930761,0.));
#7362=CARTESIAN_POINT('Origin',(0.,0.,0.));
#7363=CARTESIAN_POINT('',(-2.05,1.14891252930761,2.51052593825207E-16));
#7364=CARTESIAN_POINT('Origin',(0.,1.14891252930761,0.));
#7365=CARTESIAN_POINT('',(-2.05,1.65,-2.51052593825207E-16));
#7366=CARTESIAN_POINT('',(-2.05,0.,2.51052593825207E-16));
#7367=CARTESIAN_POINT('Origin',(0.,1.65,0.));
#7368=CARTESIAN_POINT('Origin',(0.,0.,0.));
#7369=CARTESIAN_POINT('',(-1.43895998899814E-16,-1.76221774462768E-32,-2.35));
#7370=CARTESIAN_POINT('',(-1.43895998899814E-16,-1.76221774462768E-32,2.35));
#7371=CARTESIAN_POINT('Origin',(0.,0.,0.));
#7372=CARTESIAN_POINT('Origin',(0.,1.55,-1.49));
#7373=CARTESIAN_POINT('',(-3.76384615384615,1.55,-2.13));
#7374=CARTESIAN_POINT('',(-1.81744325908679,1.55,-2.13));
#7375=CARTESIAN_POINT('',(0.,1.55,-2.13));
#7376=CARTESIAN_POINT('',(-2.46585583768694,1.55,-1.32648218523477));
#7377=CARTESIAN_POINT('',(-1.68,1.55,-0.84));
#7378=CARTESIAN_POINT('Origin',(0.,1.55,0.));
#7379=CARTESIAN_POINT('Origin',(0.,1.55,-1.49));
#7380=CARTESIAN_POINT('',(1.81744325908679,1.55,-2.13));
#7381=CARTESIAN_POINT('',(3.76384615384615,1.55,-2.13));
#7382=CARTESIAN_POINT('',(0.,1.55,-2.13));
#7383=CARTESIAN_POINT('',(2.46585583768694,1.55,-1.32648218523477));
#7384=CARTESIAN_POINT('Origin',(0.,1.55,0.));
#7385=CARTESIAN_POINT('',(3.78,1.55,-2.14));
#7386=CARTESIAN_POINT('Origin',(0.,-1.55,-1.49));
#7387=CARTESIAN_POINT('',(-1.81744325908679,-1.55,-2.13));
#7388=CARTESIAN_POINT('',(-3.76384615384615,-1.55,-2.13));
#7389=CARTESIAN_POINT('',(0.,-1.55,-2.13));
#7390=CARTESIAN_POINT('',(-2.46585583768694,-1.55,-1.32648218523477));
#7391=CARTESIAN_POINT('Origin',(0.,-1.55,0.));
#7392=CARTESIAN_POINT('',(-1.68,-1.55,-0.84));
#7393=CARTESIAN_POINT('Origin',(-3.78,0.,-2.14));
#7394=CARTESIAN_POINT('',(-3.76384615384615,0.,-2.13));
#7395=CARTESIAN_POINT('',(-2.46585583768694,0.,-1.32648218523477));
#7396=CARTESIAN_POINT('Origin',(0.,-1.55,-1.49));
#7397=CARTESIAN_POINT('',(3.76384615384615,-1.55,-2.13));
#7398=CARTESIAN_POINT('',(1.81744325908679,-1.55,-2.13));
#7399=CARTESIAN_POINT('',(0.,-1.55,-2.13));
#7400=CARTESIAN_POINT('',(2.46585583768694,-1.55,-1.32648218523477));
#7401=CARTESIAN_POINT('',(3.78,-1.55,-2.14));
#7402=CARTESIAN_POINT('Origin',(0.,-1.55,0.));
#7403=CARTESIAN_POINT('Origin',(1.68,0.,-0.84));
#7404=CARTESIAN_POINT('',(3.76384615384615,0.,-2.13));
#7405=CARTESIAN_POINT('',(2.46585583768694,0.,-1.32648218523477));
#7406=CARTESIAN_POINT('Origin',(0.,0.,-2.13));
#7407=CARTESIAN_POINT('',(-6.35,1.9,-2.13));
#7408=CARTESIAN_POINT('',(-6.35,-1.9,-2.13));
#7409=CARTESIAN_POINT('',(-6.35,1.9,-2.13));
#7410=CARTESIAN_POINT('',(6.35,-1.9,-2.13));
#7411=CARTESIAN_POINT('',(-6.35,-1.9,-2.13));
#7412=CARTESIAN_POINT('',(6.35,1.9,-2.13));
#7413=CARTESIAN_POINT('',(6.35,-1.9,-2.13));
#7414=CARTESIAN_POINT('',(6.35,1.9,-2.13));
#7415=CARTESIAN_POINT('',(4.1,7.9602041944578E-17,-2.13));
#7416=CARTESIAN_POINT('Origin',(4.75,0.,-2.13));
#7417=CARTESIAN_POINT('',(-5.4,7.9602041944578E-17,-2.13));
#7418=CARTESIAN_POINT('Origin',(-4.75,0.,-2.13));
#7419=CARTESIAN_POINT('',(1.81744325908679,-1.65,-2.13));
#7420=CARTESIAN_POINT('',(1.81744325908679,0.,-2.13));
#7421=CARTESIAN_POINT('',(-1.81744325908679,-1.65,-2.13));
#7422=CARTESIAN_POINT('',(0.,-1.65,-2.13));
#7423=CARTESIAN_POINT('',(-1.81744325908679,0.,-2.13));
#7424=CARTESIAN_POINT('',(-1.81744325908679,1.65,-2.13));
#7425=CARTESIAN_POINT('',(-1.81744325908679,0.,-2.13));
#7426=CARTESIAN_POINT('',(1.81744325908679,1.65,-2.13));
#7427=CARTESIAN_POINT('',(0.,1.65,-2.13));
#7428=CARTESIAN_POINT('',(1.81744325908679,0.,-2.13));
#7429=CARTESIAN_POINT('Origin',(0.,0.,0.));
#7430=CARTESIAN_POINT('Origin',(0.,1.65,0.));
#7431=CARTESIAN_POINT('Origin',(0.,-1.65,0.));
#7432=CARTESIAN_POINT('Origin',(0.,-1.65,0.));
#7433=CARTESIAN_POINT('Origin',(0.,1.65,0.));
#7434=CARTESIAN_POINT('Origin',(3.35,1.4,-3.33));
#7435=CARTESIAN_POINT('',(3.35,1.4,-3.33));
#7436=CARTESIAN_POINT('',(-3.35,1.4,-3.33));
#7437=CARTESIAN_POINT('',(1.675,1.4,-3.33));
#7438=CARTESIAN_POINT('',(3.35,1.4,-2.83));
#7439=CARTESIAN_POINT('',(3.35,1.4,-3.33));
#7440=CARTESIAN_POINT('',(-3.35,1.4,-2.83));
#7441=CARTESIAN_POINT('',(3.35,1.4,-2.83));
#7442=CARTESIAN_POINT('',(-3.35,1.4,-3.33));
#7443=CARTESIAN_POINT('Origin',(3.35,-1.4,-3.33));
#7444=CARTESIAN_POINT('',(3.35,-1.4,-3.33));
#7445=CARTESIAN_POINT('',(3.35,-0.7,-3.33));
#7446=CARTESIAN_POINT('',(3.35,-1.4,-2.83));
#7447=CARTESIAN_POINT('',(3.35,-1.4,-3.33));
#7448=CARTESIAN_POINT('',(3.35,-1.4,-2.83));
#7449=CARTESIAN_POINT('Origin',(-3.35,-1.4,-3.33));
#7450=CARTESIAN_POINT('',(-3.35,-1.4,-3.33));
#7451=CARTESIAN_POINT('',(-1.675,-1.4,-3.33));
#7452=CARTESIAN_POINT('',(-3.35,-1.4,-2.83));
#7453=CARTESIAN_POINT('',(-3.35,-1.4,-3.33));
#7454=CARTESIAN_POINT('',(-3.35,-1.4,-2.83));
#7455=CARTESIAN_POINT('Origin',(-3.35,1.4,-3.33));
#7456=CARTESIAN_POINT('',(-3.35,0.7,-3.33));
#7457=CARTESIAN_POINT('',(-3.35,1.4,-2.83));
#7458=CARTESIAN_POINT('Origin',(0.,0.,-2.83));
#7459=CARTESIAN_POINT('Origin',(-4.75,0.,-3.33));
#7460=CARTESIAN_POINT('',(-5.4,-7.9602041944578E-17,-3.33));
#7461=CARTESIAN_POINT('Origin',(-4.75,0.,-3.33));
#7462=CARTESIAN_POINT('',(-5.4,-7.9602041944578E-17,-3.33));
#7463=CARTESIAN_POINT('Origin',(4.75,0.,-3.33));
#7464=CARTESIAN_POINT('',(4.1,-7.9602041944578E-17,-3.33));
#7465=CARTESIAN_POINT('Origin',(4.75,0.,-3.33));
#7466=CARTESIAN_POINT('',(4.1,-7.9602041944578E-17,-3.33));
#7467=CARTESIAN_POINT('Origin',(6.35,1.9,-3.33));
#7468=CARTESIAN_POINT('',(6.35,1.9,-3.33));
#7469=CARTESIAN_POINT('',(-6.35,1.9,-3.33));
#7470=CARTESIAN_POINT('',(6.35,1.9,-3.33));
#7471=CARTESIAN_POINT('',(-6.35,1.9,-3.33));
#7472=CARTESIAN_POINT('',(6.35,1.9,-3.33));
#7473=CARTESIAN_POINT('Origin',(6.35,-1.9,-3.33));
#7474=CARTESIAN_POINT('',(6.35,-1.9,-3.33));
#7475=CARTESIAN_POINT('',(6.35,-1.9,-3.33));
#7476=CARTESIAN_POINT('',(6.35,-1.9,-3.33));
#7477=CARTESIAN_POINT('Origin',(-6.35,-1.9,-3.33));
#7478=CARTESIAN_POINT('',(-6.35,-1.9,-3.33));
#7479=CARTESIAN_POINT('',(-6.35,-1.9,-3.33));
#7480=CARTESIAN_POINT('',(-6.35,-1.9,-3.33));
#7481=CARTESIAN_POINT('Origin',(-6.35,1.9,-3.33));
#7482=CARTESIAN_POINT('',(-6.35,1.9,-3.33));
#7483=CARTESIAN_POINT('Origin',(0.,0.,-3.33));
#7484=CARTESIAN_POINT('',(0.,0.,0.));
#7485=CARTESIAN_POINT('Origin',(0.,0.,0.));
#7486=CARTESIAN_POINT('',(-1.8,-0.85,-2.20436423846524E-16));
#7487=CARTESIAN_POINT('Origin',(0.,-0.85,0.));
#7488=CARTESIAN_POINT('',(-1.8,0.85,-2.20436423846524E-16));
#7489=CARTESIAN_POINT('',(-1.8,0.,-2.20436423846524E-16));
#7490=CARTESIAN_POINT('Origin',(0.,0.85,0.));
#7491=CARTESIAN_POINT('Origin',(2.19089023002066,0.85,0.));
#7492=CARTESIAN_POINT('',(2.19089023002066,0.85,0.));
#7493=CARTESIAN_POINT('Origin',(0.,0.85,0.));
#7494=CARTESIAN_POINT('Origin',(3.99680288865056E-15,0.,0.));
#7495=CARTESIAN_POINT('',(3.85290688975075E-15,-1.76221774462768E-32,2.35));
#7496=CARTESIAN_POINT('',(3.85290688975075E-15,-1.76221774462768E-32,-2.35));
#7497=CARTESIAN_POINT('Origin',(3.99680288865056E-15,0.,0.));
#7498=CARTESIAN_POINT('',(2.19089023002066,-0.85,0.));
#7499=CARTESIAN_POINT('Origin',(0.,-0.85,0.));
#7500=CARTESIAN_POINT('Origin',(1.8,-0.85,0.));
#7501=CARTESIAN_POINT('Origin',(0.,1.55,0.));
#7502=CARTESIAN_POINT('',(1.42894191624432,1.8,0.825000000000001));
#7503=CARTESIAN_POINT('',(1.53744468918255,1.55,0.598968970568896));
#7504=CARTESIAN_POINT('Ctrl Pts',(1.42894191624432,1.8,0.825000000000001));
#7505=CARTESIAN_POINT('Ctrl Pts',(1.44466308895875,1.8,0.797770130104052));
#7506=CARTESIAN_POINT('Ctrl Pts',(1.46055812562105,1.79370633789704,0.768258557763732));
#7507=CARTESIAN_POINT('Ctrl Pts',(1.48824888379079,1.76817777258318,0.713138492740816));
#7508=CARTESIAN_POINT('Ctrl Pts',(1.50008999307766,1.74894552961493,0.687551581002689));
#7509=CARTESIAN_POINT('Ctrl Pts',(1.51812136280714,1.70460745840382,0.646764802471699));
#7510=CARTESIAN_POINT('Ctrl Pts',(1.52552758004446,1.67652816181843,0.628833667319578));
#7511=CARTESIAN_POINT('Ctrl Pts',(1.53516661651472,1.61494799959182,0.604921184808251));
#7512=CARTESIAN_POINT('Ctrl Pts',(1.53744468918255,1.58144291640553,0.598968970568896));
#7513=CARTESIAN_POINT('Ctrl Pts',(1.53744468918255,1.55,0.598968970568896));
#7514=CARTESIAN_POINT('',(1.42894191624432,1.3,0.825000000000001));
#7515=CARTESIAN_POINT('Ctrl Pts',(1.42894191624432,1.3,0.825000000000001));
#7516=CARTESIAN_POINT('Ctrl Pts',(1.4132207435299,1.3,0.852229869895949));
#7517=CARTESIAN_POINT('Ctrl Pts',(1.39561049050871,1.30629366210296,0.880751161609749));
#7518=CARTESIAN_POINT('Ctrl Pts',(1.36172049302549,1.33182222741682,0.932292094146256));
#7519=CARTESIAN_POINT('Ctrl Pts',(1.34548213209931,1.35105447038507,0.955340251466734));
#7520=CARTESIAN_POINT('Ctrl Pts',(1.31917543061769,1.39539254159618,0.99134926498299));
#7521=CARTESIAN_POINT('Ctrl Pts',(1.30734972067592,1.42347183818157,1.00672880483252));
#7522=CARTESIAN_POINT('Ctrl Pts',(1.29146042158868,1.48505200040818,1.02703269653942));
#7523=CARTESIAN_POINT('Ctrl Pts',(1.28744468918255,1.51855708359447,1.03198167246111));
#7524=CARTESIAN_POINT('Ctrl Pts',(1.28744468918255,1.58144291640553,1.03198167246111));
#7525=CARTESIAN_POINT('Ctrl Pts',(1.29146042158868,1.61494799959182,1.02703269653942));
#7526=CARTESIAN_POINT('Ctrl Pts',(1.30734972067592,1.67652816181843,1.00672880483252));
#7527=CARTESIAN_POINT('Ctrl Pts',(1.31917543061769,1.70460745840382,0.991349264982991));
#7528=CARTESIAN_POINT('Ctrl Pts',(1.34548213209931,1.74894552961493,0.955340251466735));
#7529=CARTESIAN_POINT('Ctrl Pts',(1.36172049302549,1.76817777258318,0.932292094146256));
#7530=CARTESIAN_POINT('Ctrl Pts',(1.39561049050871,1.79370633789704,0.880751161609749));
#7531=CARTESIAN_POINT('Ctrl Pts',(1.4132207435299,1.8,0.85222986989595));
#7532=CARTESIAN_POINT('Ctrl Pts',(1.42894191624432,1.8,0.825000000000001));
#7533=CARTESIAN_POINT('Ctrl Pts',(1.53744468918255,1.55,0.598968970568896));
#7534=CARTESIAN_POINT('Ctrl Pts',(1.53744468918255,1.51855708359447,0.598968970568896));
#7535=CARTESIAN_POINT('Ctrl Pts',(1.53516661651472,1.48505200040818,0.60492118480825));
#7536=CARTESIAN_POINT('Ctrl Pts',(1.52552758004446,1.42347183818157,0.628833667319578));
#7537=CARTESIAN_POINT('Ctrl Pts',(1.51812136280714,1.39539254159618,0.646764802471699));
#7538=CARTESIAN_POINT('Ctrl Pts',(1.50008999307766,1.35105447038507,0.687551581002689));
#7539=CARTESIAN_POINT('Ctrl Pts',(1.48824888379079,1.33182222741682,0.713138492740816));
#7540=CARTESIAN_POINT('Ctrl Pts',(1.46055812562105,1.30629366210296,0.768258557763732));
#7541=CARTESIAN_POINT('Ctrl Pts',(1.44466308895875,1.3,0.797770130104052));
#7542=CARTESIAN_POINT('Ctrl Pts',(1.42894191624432,1.3,0.825000000000001));
#7543=CARTESIAN_POINT('',(0.963525491562421,1.55,0.267616567329818));
#7544=CARTESIAN_POINT('',(0.125,1.55,-0.21650635094611));
#7545=CARTESIAN_POINT('Ctrl Pts',(0.963525491562421,1.55,0.267616567329818));
#7546=CARTESIAN_POINT('Ctrl Pts',(0.963525491562421,1.5815373526696,0.267616567329818));
#7547=CARTESIAN_POINT('Ctrl Pts',(0.961833761492987,1.61508042700263,0.273949373987484));
#7548=CARTESIAN_POINT('Ctrl Pts',(0.954308486908894,1.67663267125761,0.299111603474268));
#7549=CARTESIAN_POINT('Ctrl Pts',(0.948394987258249,1.70465411363682,0.31788699900678));
#7550=CARTESIAN_POINT('Ctrl Pts',(0.933155485613026,1.74889618382539,0.360174810895352));
#7551=CARTESIAN_POINT('Ctrl Pts',(0.92278792026947,1.76811531482682,0.386546956384144));
#7552=CARTESIAN_POINT('Ctrl Pts',(0.897143218189782,1.79367084275751,0.442820664919227));
#7553=CARTESIAN_POINT('Ctrl Pts',(0.881791875377343,1.8,0.472691670144998));
#7554=CARTESIAN_POINT('Ctrl Pts',(0.850258932191534,1.8,0.527308329855003));
#7555=CARTESIAN_POINT('Ctrl Pts',(0.832065554235658,1.79367084275751,0.555538485325664));
#7556=CARTESIAN_POINT('Ctrl Pts',(0.796153444118959,1.76811531482682,0.605884303066698));
#7557=CARTESIAN_POINT('Ctrl Pts',(0.778498278845144,1.74889618382539,0.62804895077401));
#7558=CARTESIAN_POINT('Ctrl Pts',(0.749495710301794,1.70465411363682,0.662390652284073));
#7559=CARTESIAN_POINT('Ctrl Pts',(0.73619249062986,1.67663267125761,0.676899590973058));
#7560=CARTESIAN_POINT('Ctrl Pts',(0.718163997970498,1.61508042700263,0.695997784676728));
#7561=CARTESIAN_POINT('Ctrl Pts',(0.713525491562421,1.5815373526696,0.700629269222037));
#7562=CARTESIAN_POINT('Ctrl Pts',(0.713525491562421,1.5184626473304,0.700629269222037));
#7563=CARTESIAN_POINT('Ctrl Pts',(0.718163997970498,1.48491957299737,0.695997784676728));
#7564=CARTESIAN_POINT('Ctrl Pts',(0.73619249062986,1.42336732874239,0.676899590973058));
#7565=CARTESIAN_POINT('Ctrl Pts',(0.749495710301794,1.39534588636318,0.662390652284073));
#7566=CARTESIAN_POINT('Ctrl Pts',(0.778498278845144,1.35110381617461,0.62804895077401));
#7567=CARTESIAN_POINT('Ctrl Pts',(0.796153444118959,1.33188468517318,0.605884303066698));
#7568=CARTESIAN_POINT('Ctrl Pts',(0.832065554235658,1.30632915724249,0.555538485325664));
#7569=CARTESIAN_POINT('Ctrl Pts',(0.850258932191534,1.3,0.527308329855003));
#7570=CARTESIAN_POINT('Ctrl Pts',(0.881791875377343,1.3,0.472691670144998));
#7571=CARTESIAN_POINT('Ctrl Pts',(0.897143218189782,1.30632915724249,0.442820664919227));
#7572=CARTESIAN_POINT('Ctrl Pts',(0.92278792026947,1.33188468517318,0.386546956384144));
#7573=CARTESIAN_POINT('Ctrl Pts',(0.933155485613026,1.35110381617461,0.360174810895352));
#7574=CARTESIAN_POINT('Ctrl Pts',(0.948394987258249,1.39534588636318,0.31788699900678));
#7575=CARTESIAN_POINT('Ctrl Pts',(0.954308486908894,1.42336732874239,0.299111603474268));
#7576=CARTESIAN_POINT('Ctrl Pts',(0.961833761492987,1.48491957299738,0.273949373987484));
#7577=CARTESIAN_POINT('Ctrl Pts',(0.963525491562421,1.5184626473304,0.267616567329818));
#7578=CARTESIAN_POINT('Ctrl Pts',(0.963525491562421,1.55,0.267616567329818));
#7579=CARTESIAN_POINT('Origin',(0.,1.55,0.));
#7580=CARTESIAN_POINT('',(-0.713525491562421,1.55,-0.700629269222037));
#7581=CARTESIAN_POINT('Ctrl Pts',(-0.713525491562421,1.55,-0.700629269222037));
#7582=CARTESIAN_POINT('Ctrl Pts',(-0.713525491562421,1.5184626473304,-0.700629269222037));
#7583=CARTESIAN_POINT('Ctrl Pts',(-0.718163997970498,1.48491957299737,-0.695997784676728));
#7584=CARTESIAN_POINT('Ctrl Pts',(-0.73619249062986,1.42336732874239,-0.676899590973058));
#7585=CARTESIAN_POINT('Ctrl Pts',(-0.749495710301794,1.39534588636318,-0.662390652284073));
#7586=CARTESIAN_POINT('Ctrl Pts',(-0.778498278845144,1.35110381617461,-0.62804895077401));
#7587=CARTESIAN_POINT('Ctrl Pts',(-0.796153444118959,1.33188468517318,-0.605884303066698));
#7588=CARTESIAN_POINT('Ctrl Pts',(-0.832065554235658,1.30632915724249,-0.555538485325664));
#7589=CARTESIAN_POINT('Ctrl Pts',(-0.850258932191534,1.3,-0.527308329855003));
#7590=CARTESIAN_POINT('Ctrl Pts',(-0.881791875377343,1.3,-0.472691670144998));
#7591=CARTESIAN_POINT('Ctrl Pts',(-0.897143218189782,1.30632915724249,-0.442820664919227));
#7592=CARTESIAN_POINT('Ctrl Pts',(-0.92278792026947,1.33188468517318,-0.386546956384144));
#7593=CARTESIAN_POINT('Ctrl Pts',(-0.933155485613026,1.35110381617461,-0.360174810895352));
#7594=CARTESIAN_POINT('Ctrl Pts',(-0.948394987258249,1.39534588636318,-0.31788699900678));
#7595=CARTESIAN_POINT('Ctrl Pts',(-0.954308486908894,1.42336732874239,-0.299111603474268));
#7596=CARTESIAN_POINT('Ctrl Pts',(-0.961833761492986,1.48491957299737,-0.273949373987484));
#7597=CARTESIAN_POINT('Ctrl Pts',(-0.963525491562421,1.5184626473304,-0.267616567329818));
#7598=CARTESIAN_POINT('Ctrl Pts',(-0.963525491562421,1.5815373526696,-0.267616567329818));
#7599=CARTESIAN_POINT('Ctrl Pts',(-0.961833761492986,1.61508042700263,-0.273949373987484));
#7600=CARTESIAN_POINT('Ctrl Pts',(-0.954308486908894,1.67663267125761,-0.299111603474268));
#7601=CARTESIAN_POINT('Ctrl Pts',(-0.948394987258249,1.70465411363682,-0.31788699900678));
#7602=CARTESIAN_POINT('Ctrl Pts',(-0.933155485613026,1.74889618382539,-0.360174810895352));
#7603=CARTESIAN_POINT('Ctrl Pts',(-0.92278792026947,1.76811531482682,-0.386546956384144));
#7604=CARTESIAN_POINT('Ctrl Pts',(-0.897143218189782,1.79367084275751,-0.442820664919227));
#7605=CARTESIAN_POINT('Ctrl Pts',(-0.881791875377343,1.8,-0.472691670144998));
#7606=CARTESIAN_POINT('Ctrl Pts',(-0.850258932191534,1.8,-0.527308329855003));
#7607=CARTESIAN_POINT('Ctrl Pts',(-0.832065554235658,1.79367084275751,-0.555538485325664));
#7608=CARTESIAN_POINT('Ctrl Pts',(-0.796153444118959,1.76811531482682,-0.605884303066698));
#7609=CARTESIAN_POINT('Ctrl Pts',(-0.778498278845144,1.74889618382539,-0.62804895077401));
#7610=CARTESIAN_POINT('Ctrl Pts',(-0.749495710301794,1.70465411363682,-0.662390652284073));
#7611=CARTESIAN_POINT('Ctrl Pts',(-0.73619249062986,1.67663267125761,-0.676899590973058));
#7612=CARTESIAN_POINT('Ctrl Pts',(-0.718163997970498,1.61508042700263,-0.695997784676728));
#7613=CARTESIAN_POINT('Ctrl Pts',(-0.713525491562421,1.5815373526696,-0.700629269222037));
#7614=CARTESIAN_POINT('Ctrl Pts',(-0.713525491562421,1.55,-0.700629269222037));
#7615=CARTESIAN_POINT('',(-1.28744468918255,1.55,-1.03198167246111));
#7616=CARTESIAN_POINT('',(0.125,1.55,-0.21650635094611));
#7617=CARTESIAN_POINT('',(-1.42894191624432,1.3,-0.825000000000001));
#7618=CARTESIAN_POINT('Ctrl Pts',(-1.42894191624432,1.3,-0.825000000000001));
#7619=CARTESIAN_POINT('Ctrl Pts',(-1.4132207435299,1.3,-0.852229869895949));
#7620=CARTESIAN_POINT('Ctrl Pts',(-1.39561049050871,1.30629366210296,-0.880751161609749));
#7621=CARTESIAN_POINT('Ctrl Pts',(-1.36172049302549,1.33182222741682,-0.932292094146256));
#7622=CARTESIAN_POINT('Ctrl Pts',(-1.34548213209931,1.35105447038507,-0.955340251466735));
#7623=CARTESIAN_POINT('Ctrl Pts',(-1.31917543061769,1.39539254159618,-0.991349264982991));
#7624=CARTESIAN_POINT('Ctrl Pts',(-1.30734972067592,1.42347183818157,-1.00672880483252));
#7625=CARTESIAN_POINT('Ctrl Pts',(-1.29146042158868,1.48505200040818,-1.02703269653942));
#7626=CARTESIAN_POINT('Ctrl Pts',(-1.28744468918255,1.51855708359447,-1.03198167246111));
#7627=CARTESIAN_POINT('Ctrl Pts',(-1.28744468918255,1.55,-1.03198167246111));
#7628=CARTESIAN_POINT('',(-1.42894191624432,1.8,-0.825000000000001));
#7629=CARTESIAN_POINT('Ctrl Pts',(-1.42894191624432,1.8,-0.825000000000001));
#7630=CARTESIAN_POINT('Ctrl Pts',(-1.44466308895875,1.8,-0.797770130104052));
#7631=CARTESIAN_POINT('Ctrl Pts',(-1.46055812562105,1.79370633789704,-0.768258557763732));
#7632=CARTESIAN_POINT('Ctrl Pts',(-1.48824888379079,1.76817777258318,-0.713138492740816));
#7633=CARTESIAN_POINT('Ctrl Pts',(-1.50008999307766,1.74894552961493,-0.687551581002689));
#7634=CARTESIAN_POINT('Ctrl Pts',(-1.51812136280714,1.70460745840382,-0.646764802471699));
#7635=CARTESIAN_POINT('Ctrl Pts',(-1.52552758004446,1.67652816181843,-0.628833667319578));
#7636=CARTESIAN_POINT('Ctrl Pts',(-1.53516661651472,1.61494799959182,-0.60492118480825));
#7637=CARTESIAN_POINT('Ctrl Pts',(-1.53744468918255,1.58144291640553,-0.598968970568896));
#7638=CARTESIAN_POINT('Ctrl Pts',(-1.53744468918255,1.51855708359447,-0.598968970568896));
#7639=CARTESIAN_POINT('Ctrl Pts',(-1.53516661651472,1.48505200040818,-0.60492118480825));
#7640=CARTESIAN_POINT('Ctrl Pts',(-1.52552758004446,1.42347183818157,-0.628833667319578));
#7641=CARTESIAN_POINT('Ctrl Pts',(-1.51812136280714,1.39539254159618,-0.646764802471699));
#7642=CARTESIAN_POINT('Ctrl Pts',(-1.50008999307766,1.35105447038507,-0.687551581002689));
#7643=CARTESIAN_POINT('Ctrl Pts',(-1.48824888379079,1.33182222741682,-0.713138492740816));
#7644=CARTESIAN_POINT('Ctrl Pts',(-1.46055812562105,1.30629366210296,-0.768258557763732));
#7645=CARTESIAN_POINT('Ctrl Pts',(-1.44466308895875,1.3,-0.797770130104052));
#7646=CARTESIAN_POINT('Ctrl Pts',(-1.42894191624432,1.3,-0.825000000000001));
#7647=CARTESIAN_POINT('Ctrl Pts',(-1.28744468918255,1.55,-1.03198167246111));
#7648=CARTESIAN_POINT('Ctrl Pts',(-1.28744468918255,1.58144291640553,-1.03198167246111));
#7649=CARTESIAN_POINT('Ctrl Pts',(-1.29146042158868,1.61494799959182,-1.02703269653942));
#7650=CARTESIAN_POINT('Ctrl Pts',(-1.30734972067592,1.67652816181843,-1.00672880483252));
#7651=CARTESIAN_POINT('Ctrl Pts',(-1.31917543061769,1.70460745840382,-0.991349264982991));
#7652=CARTESIAN_POINT('Ctrl Pts',(-1.34548213209931,1.74894552961493,-0.955340251466734));
#7653=CARTESIAN_POINT('Ctrl Pts',(-1.36172049302549,1.76817777258318,-0.932292094146256));
#7654=CARTESIAN_POINT('Ctrl Pts',(-1.39561049050871,1.79370633789704,-0.880751161609749));
#7655=CARTESIAN_POINT('Ctrl Pts',(-1.4132207435299,1.8,-0.852229869895949));
#7656=CARTESIAN_POINT('Ctrl Pts',(-1.42894191624432,1.8,-0.825000000000001));
#7657=CARTESIAN_POINT('Origin',(0.,1.55,0.));
#7658=CARTESIAN_POINT('',(-1.65,0.85,-2.02066721859313E-16));
#7659=CARTESIAN_POINT('Origin',(0.,0.85,0.));
#7660=CARTESIAN_POINT('',(-1.65,2.25,-2.02066721859313E-16));
#7661=CARTESIAN_POINT('',(-1.65,1.55,-2.02066721859313E-16));
#7662=CARTESIAN_POINT('Origin',(0.,2.25,0.));
#7663=CARTESIAN_POINT('',(-1.42894191624432,1.3,0.825));
#7664=CARTESIAN_POINT('',(-1.42894191624432,1.8,0.825));
#7665=CARTESIAN_POINT('Ctrl Pts',(-1.42894191624432,1.3,0.825));
#7666=CARTESIAN_POINT('Ctrl Pts',(-1.44466308895875,1.3,0.797770130104051));
#7667=CARTESIAN_POINT('Ctrl Pts',(-1.46055812562105,1.30629366210296,0.768258557763731));
#7668=CARTESIAN_POINT('Ctrl Pts',(-1.48824888379079,1.33182222741682,0.713138492740815));
#7669=CARTESIAN_POINT('Ctrl Pts',(-1.50008999307766,1.35105447038507,0.687551581002688));
#7670=CARTESIAN_POINT('Ctrl Pts',(-1.51812136280714,1.39539254159618,0.646764802471698));
#7671=CARTESIAN_POINT('Ctrl Pts',(-1.52552758004446,1.42347183818157,0.628833667319577));
#7672=CARTESIAN_POINT('Ctrl Pts',(-1.53516661651472,1.48505200040818,0.604921184808249));
#7673=CARTESIAN_POINT('Ctrl Pts',(-1.53744468918255,1.51855708359447,0.598968970568895));
#7674=CARTESIAN_POINT('Ctrl Pts',(-1.53744468918255,1.58144291640553,0.598968970568895));
#7675=CARTESIAN_POINT('Ctrl Pts',(-1.53516661651472,1.61494799959182,0.604921184808249));
#7676=CARTESIAN_POINT('Ctrl Pts',(-1.52552758004446,1.67652816181843,0.628833667319577));
#7677=CARTESIAN_POINT('Ctrl Pts',(-1.51812136280714,1.70460745840382,0.646764802471698));
#7678=CARTESIAN_POINT('Ctrl Pts',(-1.50008999307766,1.74894552961493,0.687551581002688));
#7679=CARTESIAN_POINT('Ctrl Pts',(-1.48824888379079,1.76817777258318,0.713138492740815));
#7680=CARTESIAN_POINT('Ctrl Pts',(-1.46055812562105,1.79370633789704,0.768258557763731));
#7681=CARTESIAN_POINT('Ctrl Pts',(-1.44466308895875,1.8,0.797770130104051));
#7682=CARTESIAN_POINT('Ctrl Pts',(-1.42894191624432,1.8,0.825));
#7683=CARTESIAN_POINT('',(-1.28744468918255,1.55,1.03198167246111));
#7684=CARTESIAN_POINT('Ctrl Pts',(-1.42894191624432,1.8,0.825));
#7685=CARTESIAN_POINT('Ctrl Pts',(-1.4132207435299,1.8,0.852229869895948));
#7686=CARTESIAN_POINT('Ctrl Pts',(-1.39561049050871,1.79370633789704,0.880751161609747));
#7687=CARTESIAN_POINT('Ctrl Pts',(-1.36172049302549,1.76817777258318,0.932292094146255));
#7688=CARTESIAN_POINT('Ctrl Pts',(-1.34548213209931,1.74894552961493,0.955340251466733));
#7689=CARTESIAN_POINT('Ctrl Pts',(-1.31917543061769,1.70460745840382,0.991349264982989));
#7690=CARTESIAN_POINT('Ctrl Pts',(-1.30734972067592,1.67652816181843,1.00672880483252));
#7691=CARTESIAN_POINT('Ctrl Pts',(-1.29146042158868,1.61494799959182,1.02703269653942));
#7692=CARTESIAN_POINT('Ctrl Pts',(-1.28744468918255,1.58144291640553,1.03198167246111));
#7693=CARTESIAN_POINT('Ctrl Pts',(-1.28744468918255,1.55,1.03198167246111));
#7694=CARTESIAN_POINT('Ctrl Pts',(-1.28744468918255,1.55,1.03198167246111));
#7695=CARTESIAN_POINT('Ctrl Pts',(-1.28744468918255,1.51855708359447,1.03198167246111));
#7696=CARTESIAN_POINT('Ctrl Pts',(-1.29146042158868,1.48505200040818,1.02703269653942));
#7697=CARTESIAN_POINT('Ctrl Pts',(-1.30734972067592,1.42347183818157,1.00672880483252));
#7698=CARTESIAN_POINT('Ctrl Pts',(-1.31917543061769,1.39539254159618,0.99134926498299));
#7699=CARTESIAN_POINT('Ctrl Pts',(-1.34548213209931,1.35105447038508,0.955340251466733));
#7700=CARTESIAN_POINT('Ctrl Pts',(-1.36172049302549,1.33182222741682,0.932292094146255));
#7701=CARTESIAN_POINT('Ctrl Pts',(-1.39561049050871,1.30629366210296,0.880751161609748));
#7702=CARTESIAN_POINT('Ctrl Pts',(-1.4132207435299,1.3,0.852229869895949));
#7703=CARTESIAN_POINT('Ctrl Pts',(-1.42894191624432,1.3,0.825));
#7704=CARTESIAN_POINT('',(1.42894191624432,1.8,-0.825));
#7705=CARTESIAN_POINT('',(1.42894191624432,1.3,-0.825));
#7706=CARTESIAN_POINT('Ctrl Pts',(1.42894191624432,1.8,-0.825));
#7707=CARTESIAN_POINT('Ctrl Pts',(1.4132207435299,1.8,-0.852229869895949));
#7708=CARTESIAN_POINT('Ctrl Pts',(1.39561049050871,1.79370633789704,-0.880751161609748));
#7709=CARTESIAN_POINT('Ctrl Pts',(1.36172049302549,1.76817777258318,-0.932292094146255));
#7710=CARTESIAN_POINT('Ctrl Pts',(1.34548213209931,1.74894552961493,-0.955340251466734));
#7711=CARTESIAN_POINT('Ctrl Pts',(1.31917543061769,1.70460745840382,-0.99134926498299));
#7712=CARTESIAN_POINT('Ctrl Pts',(1.30734972067592,1.67652816181843,-1.00672880483252));
#7713=CARTESIAN_POINT('Ctrl Pts',(1.29146042158868,1.61494799959182,-1.02703269653942));
#7714=CARTESIAN_POINT('Ctrl Pts',(1.28744468918255,1.58144291640553,-1.03198167246111));
#7715=CARTESIAN_POINT('Ctrl Pts',(1.28744468918255,1.51855708359447,-1.03198167246111));
#7716=CARTESIAN_POINT('Ctrl Pts',(1.29146042158868,1.48505200040818,-1.02703269653942));
#7717=CARTESIAN_POINT('Ctrl Pts',(1.30734972067592,1.42347183818157,-1.00672880483252));
#7718=CARTESIAN_POINT('Ctrl Pts',(1.31917543061769,1.39539254159618,-0.99134926498299));
#7719=CARTESIAN_POINT('Ctrl Pts',(1.34548213209931,1.35105447038507,-0.955340251466734));
#7720=CARTESIAN_POINT('Ctrl Pts',(1.36172049302549,1.33182222741682,-0.932292094146255));
#7721=CARTESIAN_POINT('Ctrl Pts',(1.39561049050871,1.30629366210296,-0.880751161609748));
#7722=CARTESIAN_POINT('Ctrl Pts',(1.4132207435299,1.3,-0.852229869895948));
#7723=CARTESIAN_POINT('Ctrl Pts',(1.42894191624432,1.3,-0.825));
#7724=CARTESIAN_POINT('',(1.53744468918255,1.55,-0.598968970568895));
#7725=CARTESIAN_POINT('Ctrl Pts',(1.42894191624432,1.3,-0.825));
#7726=CARTESIAN_POINT('Ctrl Pts',(1.44466308895875,1.3,-0.797770130104051));
#7727=CARTESIAN_POINT('Ctrl Pts',(1.46055812562105,1.30629366210296,-0.768258557763731));
#7728=CARTESIAN_POINT('Ctrl Pts',(1.48824888379079,1.33182222741682,-0.713138492740815));
#7729=CARTESIAN_POINT('Ctrl Pts',(1.50008999307766,1.35105447038507,-0.687551581002688));
#7730=CARTESIAN_POINT('Ctrl Pts',(1.51812136280714,1.39539254159618,-0.646764802471698));
#7731=CARTESIAN_POINT('Ctrl Pts',(1.52552758004446,1.42347183818157,-0.628833667319577));
#7732=CARTESIAN_POINT('Ctrl Pts',(1.53516661651472,1.48505200040818,-0.604921184808249));
#7733=CARTESIAN_POINT('Ctrl Pts',(1.53744468918255,1.51855708359447,-0.598968970568895));
#7734=CARTESIAN_POINT('Ctrl Pts',(1.53744468918255,1.55,-0.598968970568895));
#7735=CARTESIAN_POINT('Ctrl Pts',(1.53744468918255,1.55,-0.598968970568895));
#7736=CARTESIAN_POINT('Ctrl Pts',(1.53744468918255,1.58144291640553,-0.598968970568895));
#7737=CARTESIAN_POINT('Ctrl Pts',(1.53516661651472,1.61494799959182,-0.604921184808249));
#7738=CARTESIAN_POINT('Ctrl Pts',(1.52552758004446,1.67652816181843,-0.628833667319577));
#7739=CARTESIAN_POINT('Ctrl Pts',(1.51812136280714,1.70460745840382,-0.646764802471698));
#7740=CARTESIAN_POINT('Ctrl Pts',(1.50008999307766,1.74894552961493,-0.687551581002688));
#7741=CARTESIAN_POINT('Ctrl Pts',(1.48824888379079,1.76817777258318,-0.713138492740815));
#7742=CARTESIAN_POINT('Ctrl Pts',(1.46055812562105,1.79370633789704,-0.768258557763731));
#7743=CARTESIAN_POINT('Ctrl Pts',(1.44466308895875,1.8,-0.797770130104051));
#7744=CARTESIAN_POINT('Ctrl Pts',(1.42894191624432,1.8,-0.825));
#7745=CARTESIAN_POINT('',(0.,1.3,-1.65));
#7746=CARTESIAN_POINT('',(0.,1.8,-1.65));
#7747=CARTESIAN_POINT('Ctrl Pts',(1.38777878078145E-17,1.3,-1.65));
#7748=CARTESIAN_POINT('Ctrl Pts',(0.0314423454288489,1.3,-1.65));
#7749=CARTESIAN_POINT('Ctrl Pts',(0.0649476351123396,1.30629366210296,-1.64900971937348));
#7750=CARTESIAN_POINT('Ctrl Pts',(0.126528390765307,1.33182222741682,-1.64543058688707));
#7751=CARTESIAN_POINT('Ctrl Pts',(0.154607860978348,1.35105447038507,-1.64289183246942));
#7752=CARTESIAN_POINT('Ctrl Pts',(0.198945932189457,1.39539254159618,-1.63811406745469));
#7753=CARTESIAN_POINT('Ctrl Pts',(0.218177859368546,1.42347183818157,-1.63556247215209));
#7754=CARTESIAN_POINT('Ctrl Pts',(0.243706194926033,1.48505200040818,-1.63195388134767));
#7755=CARTESIAN_POINT('Ctrl Pts',(0.25,1.51855708359447,-1.63095064303001));
#7756=CARTESIAN_POINT('Ctrl Pts',(0.25,1.58144291640553,-1.63095064303001));
#7757=CARTESIAN_POINT('Ctrl Pts',(0.243706194926033,1.61494799959182,-1.63195388134767));
#7758=CARTESIAN_POINT('Ctrl Pts',(0.218177859368546,1.67652816181843,-1.63556247215209));
#7759=CARTESIAN_POINT('Ctrl Pts',(0.198945932189457,1.70460745840382,-1.63811406745469));
#7760=CARTESIAN_POINT('Ctrl Pts',(0.154607860978349,1.74894552961493,-1.64289183246942));
#7761=CARTESIAN_POINT('Ctrl Pts',(0.126528390765307,1.76817777258318,-1.64543058688707));
#7762=CARTESIAN_POINT('Ctrl Pts',(0.0649476351123398,1.79370633789704,-1.64900971937348));
#7763=CARTESIAN_POINT('Ctrl Pts',(0.031442345428849,1.8,-1.65));
#7764=CARTESIAN_POINT('Ctrl Pts',(7.63278329429795E-17,1.8,-1.65));
#7765=CARTESIAN_POINT('',(-0.25,1.55,-1.63095064303001));
#7766=CARTESIAN_POINT('Ctrl Pts',(9.0205620750794E-17,1.8,-1.65));
#7767=CARTESIAN_POINT('Ctrl Pts',(-0.0314423454288488,1.8,-1.65));
#7768=CARTESIAN_POINT('Ctrl Pts',(-0.0649476351123396,1.79370633789704,
-1.64900971937348));
#7769=CARTESIAN_POINT('Ctrl Pts',(-0.126528390765307,1.76817777258318,-1.64543058688707));
#7770=CARTESIAN_POINT('Ctrl Pts',(-0.154607860978348,1.74894552961493,-1.64289183246942));
#7771=CARTESIAN_POINT('Ctrl Pts',(-0.198945932189456,1.70460745840382,-1.63811406745469));
#7772=CARTESIAN_POINT('Ctrl Pts',(-0.218177859368546,1.67652816181843,-1.63556247215209));
#7773=CARTESIAN_POINT('Ctrl Pts',(-0.243706194926033,1.61494799959182,-1.63195388134767));
#7774=CARTESIAN_POINT('Ctrl Pts',(-0.25,1.58144291640553,-1.63095064303001));
#7775=CARTESIAN_POINT('Ctrl Pts',(-0.25,1.55,-1.63095064303001));
#7776=CARTESIAN_POINT('Ctrl Pts',(-0.25,1.55,-1.63095064303001));
#7777=CARTESIAN_POINT('Ctrl Pts',(-0.25,1.51855708359447,-1.63095064303001));
#7778=CARTESIAN_POINT('Ctrl Pts',(-0.243706194926033,1.48505200040818,-1.63195388134767));
#7779=CARTESIAN_POINT('Ctrl Pts',(-0.218177859368546,1.42347183818157,-1.63556247215209));
#7780=CARTESIAN_POINT('Ctrl Pts',(-0.198945932189457,1.39539254159618,-1.63811406745469));
#7781=CARTESIAN_POINT('Ctrl Pts',(-0.154607860978349,1.35105447038507,-1.64289183246942));
#7782=CARTESIAN_POINT('Ctrl Pts',(-0.126528390765307,1.33182222741682,-1.64543058688707));
#7783=CARTESIAN_POINT('Ctrl Pts',(-0.0649476351123398,1.30629366210296,
-1.64900971937348));
#7784=CARTESIAN_POINT('Ctrl Pts',(-0.031442345428849,1.3,-1.65));
#7785=CARTESIAN_POINT('Ctrl Pts',(-4.85722573273506E-17,1.3,-1.65));
#7786=CARTESIAN_POINT('',(0.,1.8,1.65));
#7787=CARTESIAN_POINT('',(0.,1.3,1.65));
#7788=CARTESIAN_POINT('Ctrl Pts',(8.32667268468867E-17,1.8,1.65));
#7789=CARTESIAN_POINT('Ctrl Pts',(0.031442345428849,1.8,1.65));
#7790=CARTESIAN_POINT('Ctrl Pts',(0.0649476351123398,1.79370633789704,1.64900971937348));
#7791=CARTESIAN_POINT('Ctrl Pts',(0.126528390765307,1.76817777258318,1.64543058688707));
#7792=CARTESIAN_POINT('Ctrl Pts',(0.154607860978349,1.74894552961493,1.64289183246942));
#7793=CARTESIAN_POINT('Ctrl Pts',(0.198945932189457,1.70460745840382,1.63811406745469));
#7794=CARTESIAN_POINT('Ctrl Pts',(0.218177859368546,1.67652816181843,1.63556247215209));
#7795=CARTESIAN_POINT('Ctrl Pts',(0.243706194926033,1.61494799959182,1.63195388134767));
#7796=CARTESIAN_POINT('Ctrl Pts',(0.25,1.58144291640553,1.63095064303001));
#7797=CARTESIAN_POINT('Ctrl Pts',(0.25,1.51855708359447,1.63095064303001));
#7798=CARTESIAN_POINT('Ctrl Pts',(0.243706194926033,1.48505200040818,1.63195388134767));
#7799=CARTESIAN_POINT('Ctrl Pts',(0.218177859368546,1.42347183818157,1.63556247215209));
#7800=CARTESIAN_POINT('Ctrl Pts',(0.198945932189457,1.39539254159618,1.63811406745469));
#7801=CARTESIAN_POINT('Ctrl Pts',(0.154607860978348,1.35105447038507,1.64289183246942));
#7802=CARTESIAN_POINT('Ctrl Pts',(0.126528390765307,1.33182222741682,1.64543058688707));
#7803=CARTESIAN_POINT('Ctrl Pts',(0.0649476351123397,1.30629366210296,1.64900971937348));
#7804=CARTESIAN_POINT('Ctrl Pts',(0.0314423454288488,1.3,1.65));
#7805=CARTESIAN_POINT('Ctrl Pts',(-1.38777878078145E-17,1.3,1.65));
#7806=CARTESIAN_POINT('',(-0.25,1.55,1.63095064303001));
#7807=CARTESIAN_POINT('Ctrl Pts',(-5.55111512312578E-17,1.3,1.65));
#7808=CARTESIAN_POINT('Ctrl Pts',(-0.031442345428849,1.3,1.65));
#7809=CARTESIAN_POINT('Ctrl Pts',(-0.0649476351123398,1.30629366210296,
1.64900971937348));
#7810=CARTESIAN_POINT('Ctrl Pts',(-0.126528390765307,1.33182222741682,1.64543058688707));
#7811=CARTESIAN_POINT('Ctrl Pts',(-0.154607860978349,1.35105447038507,1.64289183246942));
#7812=CARTESIAN_POINT('Ctrl Pts',(-0.198945932189457,1.39539254159618,1.63811406745469));
#7813=CARTESIAN_POINT('Ctrl Pts',(-0.218177859368546,1.42347183818157,1.63556247215209));
#7814=CARTESIAN_POINT('Ctrl Pts',(-0.243706194926033,1.48505200040818,1.63195388134767));
#7815=CARTESIAN_POINT('Ctrl Pts',(-0.25,1.51855708359447,1.63095064303001));
#7816=CARTESIAN_POINT('Ctrl Pts',(-0.25,1.55,1.63095064303001));
#7817=CARTESIAN_POINT('Ctrl Pts',(-0.25,1.55,1.63095064303001));
#7818=CARTESIAN_POINT('Ctrl Pts',(-0.25,1.58144291640553,1.63095064303001));
#7819=CARTESIAN_POINT('Ctrl Pts',(-0.243706194926033,1.61494799959182,1.63195388134767));
#7820=CARTESIAN_POINT('Ctrl Pts',(-0.218177859368546,1.67652816181843,1.63556247215209));
#7821=CARTESIAN_POINT('Ctrl Pts',(-0.198945932189456,1.70460745840382,1.63811406745469));
#7822=CARTESIAN_POINT('Ctrl Pts',(-0.154607860978348,1.74894552961493,1.64289183246942));
#7823=CARTESIAN_POINT('Ctrl Pts',(-0.126528390765307,1.76817777258318,1.64543058688707));
#7824=CARTESIAN_POINT('Ctrl Pts',(-0.0649476351123396,1.79370633789704,
1.64900971937348));
#7825=CARTESIAN_POINT('Ctrl Pts',(-0.0314423454288488,1.8,1.65));
#7826=CARTESIAN_POINT('Ctrl Pts',(7.63278329429795E-17,1.8,1.65));
#7827=CARTESIAN_POINT('Origin',(0.,1.55,0.));
#7828=CARTESIAN_POINT('',(-0.713525491562421,1.55,0.700629269222037));
#7829=CARTESIAN_POINT('',(0.125,1.55,0.21650635094611));
#7830=CARTESIAN_POINT('Ctrl Pts',(-0.713525491562421,1.55,0.700629269222037));
#7831=CARTESIAN_POINT('Ctrl Pts',(-0.713525491562421,1.5815373526696,0.700629269222037));
#7832=CARTESIAN_POINT('Ctrl Pts',(-0.718163997970498,1.61508042700263,0.695997784676727));
#7833=CARTESIAN_POINT('Ctrl Pts',(-0.73619249062986,1.67663267125761,0.676899590973058));
#7834=CARTESIAN_POINT('Ctrl Pts',(-0.749495710301795,1.70465411363682,0.662390652284073));
#7835=CARTESIAN_POINT('Ctrl Pts',(-0.778498278845144,1.74889618382539,0.628048950774009));
#7836=CARTESIAN_POINT('Ctrl Pts',(-0.796153444118959,1.76811531482682,0.605884303066698));
#7837=CARTESIAN_POINT('Ctrl Pts',(-0.832065554235658,1.79367084275751,0.555538485325663));
#7838=CARTESIAN_POINT('Ctrl Pts',(-0.850258932191534,1.8,0.527308329855002));
#7839=CARTESIAN_POINT('Ctrl Pts',(-0.881791875377343,1.8,0.472691670144998));
#7840=CARTESIAN_POINT('Ctrl Pts',(-0.897143218189782,1.79367084275751,0.442820664919227));
#7841=CARTESIAN_POINT('Ctrl Pts',(-0.92278792026947,1.76811531482682,0.386546956384144));
#7842=CARTESIAN_POINT('Ctrl Pts',(-0.933155485613026,1.74889618382539,0.360174810895352));
#7843=CARTESIAN_POINT('Ctrl Pts',(-0.948394987258249,1.70465411363682,0.31788699900678));
#7844=CARTESIAN_POINT('Ctrl Pts',(-0.954308486908894,1.67663267125761,0.299111603474267));
#7845=CARTESIAN_POINT('Ctrl Pts',(-0.961833761492987,1.61508042700263,0.273949373987484));
#7846=CARTESIAN_POINT('Ctrl Pts',(-0.963525491562421,1.5815373526696,0.267616567329817));
#7847=CARTESIAN_POINT('Ctrl Pts',(-0.963525491562421,1.5184626473304,0.267616567329817));
#7848=CARTESIAN_POINT('Ctrl Pts',(-0.961833761492987,1.48491957299737,0.273949373987484));
#7849=CARTESIAN_POINT('Ctrl Pts',(-0.954308486908894,1.42336732874239,0.299111603474267));
#7850=CARTESIAN_POINT('Ctrl Pts',(-0.948394987258249,1.39534588636318,0.31788699900678));
#7851=CARTESIAN_POINT('Ctrl Pts',(-0.933155485613026,1.35110381617461,0.360174810895352));
#7852=CARTESIAN_POINT('Ctrl Pts',(-0.92278792026947,1.33188468517318,0.386546956384144));
#7853=CARTESIAN_POINT('Ctrl Pts',(-0.897143218189782,1.30632915724249,0.442820664919227));
#7854=CARTESIAN_POINT('Ctrl Pts',(-0.881791875377343,1.3,0.472691670144998));
#7855=CARTESIAN_POINT('Ctrl Pts',(-0.850258932191534,1.3,0.527308329855002));
#7856=CARTESIAN_POINT('Ctrl Pts',(-0.832065554235658,1.30632915724249,0.555538485325663));
#7857=CARTESIAN_POINT('Ctrl Pts',(-0.796153444118959,1.33188468517318,0.605884303066698));
#7858=CARTESIAN_POINT('Ctrl Pts',(-0.778498278845144,1.35110381617461,0.628048950774009));
#7859=CARTESIAN_POINT('Ctrl Pts',(-0.749495710301795,1.39534588636318,0.662390652284073));
#7860=CARTESIAN_POINT('Ctrl Pts',(-0.73619249062986,1.42336732874239,0.676899590973058));
#7861=CARTESIAN_POINT('Ctrl Pts',(-0.718163997970498,1.48491957299737,0.695997784676727));
#7862=CARTESIAN_POINT('Ctrl Pts',(-0.713525491562421,1.5184626473304,0.700629269222037));
#7863=CARTESIAN_POINT('Ctrl Pts',(-0.713525491562421,1.55,0.700629269222037));
#7864=CARTESIAN_POINT('Origin',(0.,1.55,0.));
#7865=CARTESIAN_POINT('',(0.963525491562421,1.55,-0.267616567329817));
#7866=CARTESIAN_POINT('Ctrl Pts',(0.963525491562421,1.55,-0.267616567329817));
#7867=CARTESIAN_POINT('Ctrl Pts',(0.963525491562421,1.5184626473304,-0.267616567329817));
#7868=CARTESIAN_POINT('Ctrl Pts',(0.961833761492987,1.48491957299737,-0.273949373987484));
#7869=CARTESIAN_POINT('Ctrl Pts',(0.954308486908894,1.42336732874239,-0.299111603474267));
#7870=CARTESIAN_POINT('Ctrl Pts',(0.948394987258249,1.39534588636318,-0.31788699900678));
#7871=CARTESIAN_POINT('Ctrl Pts',(0.933155485613026,1.35110381617461,-0.360174810895352));
#7872=CARTESIAN_POINT('Ctrl Pts',(0.92278792026947,1.33188468517318,-0.386546956384144));
#7873=CARTESIAN_POINT('Ctrl Pts',(0.897143218189782,1.30632915724249,-0.442820664919227));
#7874=CARTESIAN_POINT('Ctrl Pts',(0.881791875377343,1.3,-0.472691670144998));
#7875=CARTESIAN_POINT('Ctrl Pts',(0.850258932191534,1.3,-0.527308329855002));
#7876=CARTESIAN_POINT('Ctrl Pts',(0.832065554235658,1.30632915724249,-0.555538485325663));
#7877=CARTESIAN_POINT('Ctrl Pts',(0.796153444118959,1.33188468517318,-0.605884303066698));
#7878=CARTESIAN_POINT('Ctrl Pts',(0.778498278845144,1.35110381617461,-0.628048950774009));
#7879=CARTESIAN_POINT('Ctrl Pts',(0.749495710301795,1.39534588636318,-0.662390652284073));
#7880=CARTESIAN_POINT('Ctrl Pts',(0.73619249062986,1.42336732874239,-0.676899590973058));
#7881=CARTESIAN_POINT('Ctrl Pts',(0.718163997970498,1.48491957299737,-0.695997784676727));
#7882=CARTESIAN_POINT('Ctrl Pts',(0.713525491562421,1.5184626473304,-0.700629269222037));
#7883=CARTESIAN_POINT('Ctrl Pts',(0.713525491562421,1.5815373526696,-0.700629269222037));
#7884=CARTESIAN_POINT('Ctrl Pts',(0.718163997970498,1.61508042700263,-0.695997784676727));
#7885=CARTESIAN_POINT('Ctrl Pts',(0.73619249062986,1.67663267125761,-0.676899590973058));
#7886=CARTESIAN_POINT('Ctrl Pts',(0.749495710301795,1.70465411363682,-0.662390652284073));
#7887=CARTESIAN_POINT('Ctrl Pts',(0.778498278845144,1.74889618382539,-0.628048950774009));
#7888=CARTESIAN_POINT('Ctrl Pts',(0.796153444118959,1.76811531482682,-0.605884303066698));
#7889=CARTESIAN_POINT('Ctrl Pts',(0.832065554235658,1.79367084275751,-0.555538485325663));
#7890=CARTESIAN_POINT('Ctrl Pts',(0.850258932191534,1.8,-0.527308329855002));
#7891=CARTESIAN_POINT('Ctrl Pts',(0.881791875377343,1.8,-0.472691670144998));
#7892=CARTESIAN_POINT('Ctrl Pts',(0.897143218189782,1.79367084275751,-0.442820664919227));
#7893=CARTESIAN_POINT('Ctrl Pts',(0.92278792026947,1.76811531482682,-0.386546956384144));
#7894=CARTESIAN_POINT('Ctrl Pts',(0.933155485613026,1.74889618382539,-0.360174810895352));
#7895=CARTESIAN_POINT('Ctrl Pts',(0.948394987258249,1.70465411363682,-0.31788699900678));
#7896=CARTESIAN_POINT('Ctrl Pts',(0.954308486908894,1.67663267125761,-0.299111603474267));
#7897=CARTESIAN_POINT('Ctrl Pts',(0.961833761492987,1.61508042700263,-0.273949373987484));
#7898=CARTESIAN_POINT('Ctrl Pts',(0.963525491562421,1.5815373526696,-0.267616567329817));
#7899=CARTESIAN_POINT('Ctrl Pts',(0.963525491562421,1.55,-0.267616567329817));
#7900=CARTESIAN_POINT('',(0.125,1.55,0.21650635094611));
#7901=CARTESIAN_POINT('Origin',(0.,1.55,0.));
#7902=CARTESIAN_POINT('',(-0.25,1.55,-0.968245836551854));
#7903=CARTESIAN_POINT('',(-0.25,1.55,0.));
#7904=CARTESIAN_POINT('Ctrl Pts',(-0.25,1.55,-0.968245836551854));
#7905=CARTESIAN_POINT('Ctrl Pts',(-0.25,1.5815373526696,-0.968245836551854));
#7906=CARTESIAN_POINT('Ctrl Pts',(-0.243669763522489,1.61508042700263,-0.969947158664211));
#7907=CARTESIAN_POINT('Ctrl Pts',(-0.218115996279034,1.67663267125761,-0.976011194447325));
#7908=CARTESIAN_POINT('Ctrl Pts',(-0.198899276956455,1.70465411363682,-0.980277651290853));
#7909=CARTESIAN_POINT('Ctrl Pts',(-0.154657206767882,1.74889618382539,-0.988223761669361));
#7910=CARTESIAN_POINT('Ctrl Pts',(-0.126634476150511,1.76811531482682,-0.992431259450842));
#7911=CARTESIAN_POINT('Ctrl Pts',(-0.0650776639541238,1.79367084275751,
-0.99835915024489));
#7912=CARTESIAN_POINT('Ctrl Pts',(-0.0315329431858092,1.8,-1.));
#7913=CARTESIAN_POINT('Ctrl Pts',(0.0315329431858092,1.8,-1.));
#7914=CARTESIAN_POINT('Ctrl Pts',(0.0650776639541238,1.79367084275751,-0.99835915024489));
#7915=CARTESIAN_POINT('Ctrl Pts',(0.126634476150511,1.76811531482682,-0.992431259450842));
#7916=CARTESIAN_POINT('Ctrl Pts',(0.154657206767882,1.74889618382539,-0.988223761669361));
#7917=CARTESIAN_POINT('Ctrl Pts',(0.198899276956455,1.70465411363682,-0.980277651290853));
#7918=CARTESIAN_POINT('Ctrl Pts',(0.218115996279034,1.67663267125761,-0.976011194447325));
#7919=CARTESIAN_POINT('Ctrl Pts',(0.243669763522488,1.61508042700263,-0.969947158664211));
#7920=CARTESIAN_POINT('Ctrl Pts',(0.25,1.5815373526696,-0.968245836551854));
#7921=CARTESIAN_POINT('Ctrl Pts',(0.25,1.5184626473304,-0.968245836551854));
#7922=CARTESIAN_POINT('Ctrl Pts',(0.243669763522488,1.48491957299737,-0.969947158664211));
#7923=CARTESIAN_POINT('Ctrl Pts',(0.218115996279034,1.42336732874239,-0.976011194447325));
#7924=CARTESIAN_POINT('Ctrl Pts',(0.198899276956455,1.39534588636318,-0.980277651290853));
#7925=CARTESIAN_POINT('Ctrl Pts',(0.154657206767882,1.35110381617461,-0.988223761669361));
#7926=CARTESIAN_POINT('Ctrl Pts',(0.126634476150511,1.33188468517318,-0.992431259450842));
#7927=CARTESIAN_POINT('Ctrl Pts',(0.0650776639541239,1.30632915724249,-0.99835915024489));
#7928=CARTESIAN_POINT('Ctrl Pts',(0.0315329431858092,1.3,-1.));
#7929=CARTESIAN_POINT('Ctrl Pts',(-0.0315329431858092,1.3,-1.));
#7930=CARTESIAN_POINT('Ctrl Pts',(-0.0650776639541239,1.30632915724249,
-0.99835915024489));
#7931=CARTESIAN_POINT('Ctrl Pts',(-0.126634476150511,1.33188468517318,-0.992431259450842));
#7932=CARTESIAN_POINT('Ctrl Pts',(-0.154657206767882,1.35110381617461,-0.988223761669361));
#7933=CARTESIAN_POINT('Ctrl Pts',(-0.198899276956455,1.39534588636318,-0.980277651290853));
#7934=CARTESIAN_POINT('Ctrl Pts',(-0.218115996279034,1.42336732874239,-0.976011194447325));
#7935=CARTESIAN_POINT('Ctrl Pts',(-0.243669763522489,1.48491957299737,-0.969947158664211));
#7936=CARTESIAN_POINT('Ctrl Pts',(-0.25,1.5184626473304,-0.968245836551854));
#7937=CARTESIAN_POINT('Ctrl Pts',(-0.25,1.55,-0.968245836551854));
#7938=CARTESIAN_POINT('Origin',(0.,1.55,0.));
#7939=CARTESIAN_POINT('',(-0.25,1.55,0.968245836551854));
#7940=CARTESIAN_POINT('Ctrl Pts',(-0.25,1.55,0.968245836551854));
#7941=CARTESIAN_POINT('Ctrl Pts',(-0.25,1.5184626473304,0.968245836551854));
#7942=CARTESIAN_POINT('Ctrl Pts',(-0.243669763522489,1.48491957299737,0.969947158664211));
#7943=CARTESIAN_POINT('Ctrl Pts',(-0.218115996279034,1.42336732874239,0.976011194447325));
#7944=CARTESIAN_POINT('Ctrl Pts',(-0.198899276956455,1.39534588636318,0.980277651290853));
#7945=CARTESIAN_POINT('Ctrl Pts',(-0.154657206767882,1.35110381617461,0.988223761669361));
#7946=CARTESIAN_POINT('Ctrl Pts',(-0.126634476150511,1.33188468517318,0.992431259450842));
#7947=CARTESIAN_POINT('Ctrl Pts',(-0.065077663954124,1.30632915724249,0.99835915024489));
#7948=CARTESIAN_POINT('Ctrl Pts',(-0.0315329431858092,1.3,1.));
#7949=CARTESIAN_POINT('Ctrl Pts',(0.0315329431858092,1.3,1.));
#7950=CARTESIAN_POINT('Ctrl Pts',(0.065077663954124,1.30632915724249,0.99835915024489));
#7951=CARTESIAN_POINT('Ctrl Pts',(0.126634476150511,1.33188468517318,0.992431259450842));
#7952=CARTESIAN_POINT('Ctrl Pts',(0.154657206767882,1.35110381617461,0.988223761669361));
#7953=CARTESIAN_POINT('Ctrl Pts',(0.198899276956455,1.39534588636318,0.980277651290853));
#7954=CARTESIAN_POINT('Ctrl Pts',(0.218115996279034,1.42336732874239,0.976011194447325));
#7955=CARTESIAN_POINT('Ctrl Pts',(0.243669763522488,1.48491957299737,0.969947158664211));
#7956=CARTESIAN_POINT('Ctrl Pts',(0.25,1.5184626473304,0.968245836551854));
#7957=CARTESIAN_POINT('Ctrl Pts',(0.25,1.5815373526696,0.968245836551854));
#7958=CARTESIAN_POINT('Ctrl Pts',(0.243669763522488,1.61508042700263,0.969947158664211));
#7959=CARTESIAN_POINT('Ctrl Pts',(0.218115996279034,1.67663267125761,0.976011194447325));
#7960=CARTESIAN_POINT('Ctrl Pts',(0.198899276956455,1.70465411363682,0.980277651290853));
#7961=CARTESIAN_POINT('Ctrl Pts',(0.154657206767882,1.74889618382539,0.988223761669361));
#7962=CARTESIAN_POINT('Ctrl Pts',(0.126634476150511,1.76811531482682,0.992431259450842));
#7963=CARTESIAN_POINT('Ctrl Pts',(0.0650776639541239,1.79367084275751,0.99835915024489));
#7964=CARTESIAN_POINT('Ctrl Pts',(0.0315329431858092,1.8,1.));
#7965=CARTESIAN_POINT('Ctrl Pts',(-0.0315329431858092,1.8,1.));
#7966=CARTESIAN_POINT('Ctrl Pts',(-0.0650776639541239,1.79367084275751,
0.99835915024489));
#7967=CARTESIAN_POINT('Ctrl Pts',(-0.126634476150511,1.76811531482682,0.992431259450842));
#7968=CARTESIAN_POINT('Ctrl Pts',(-0.154657206767882,1.74889618382539,0.988223761669361));
#7969=CARTESIAN_POINT('Ctrl Pts',(-0.198899276956455,1.70465411363682,0.980277651290853));
#7970=CARTESIAN_POINT('Ctrl Pts',(-0.218115996279034,1.67663267125761,0.976011194447325));
#7971=CARTESIAN_POINT('Ctrl Pts',(-0.243669763522489,1.61508042700263,0.969947158664211));
#7972=CARTESIAN_POINT('Ctrl Pts',(-0.25,1.5815373526696,0.968245836551854));
#7973=CARTESIAN_POINT('Ctrl Pts',(-0.25,1.55,0.968245836551854));
#7974=CARTESIAN_POINT('',(-0.25,1.55,0.));
#7975=CARTESIAN_POINT('Origin',(1.65,2.25,0.));
#7976=CARTESIAN_POINT('',(-1.,2.25,-1.22464679914735E-16));
#7977=CARTESIAN_POINT('Origin',(0.,2.25,0.));
#7978=CARTESIAN_POINT('Origin',(1.75,0.85,0.));
#7979=CARTESIAN_POINT('',(-1.75,0.85,-2.14313189850787E-16));
#7980=CARTESIAN_POINT('Origin',(0.,0.85,0.));
#7981=CARTESIAN_POINT('Origin',(0.,0.,0.));
#7982=CARTESIAN_POINT('',(-1.75,-0.85,-2.14313189850787E-16));
#7983=CARTESIAN_POINT('Origin',(0.,-0.85,0.));
#7984=CARTESIAN_POINT('',(-1.75,0.,-2.14313189850787E-16));
#7985=CARTESIAN_POINT('Origin',(1.,-0.85,0.));
#7986=CARTESIAN_POINT('',(-1.,-0.85,-1.22464679914735E-16));
#7987=CARTESIAN_POINT('Origin',(0.,-0.85,0.));
#7988=CARTESIAN_POINT('Origin',(0.,0.7,0.));
#7989=CARTESIAN_POINT('',(-1.,0.7,-1.22464679914735E-16));
#7990=CARTESIAN_POINT('',(0.,0.,0.));
#7991=CARTESIAN_POINT('',(0.,0.,0.));
#7992=CARTESIAN_POINT('',(0.,0.,0.));
#7993=CARTESIAN_POINT('Origin',(0.,0.,0.));
#7994=CARTESIAN_POINT('',(-0.42,0.16,5.14351655641888E-17));
#7995=CARTESIAN_POINT('Origin',(0.,0.16,0.));
#7996=CARTESIAN_POINT('',(-0.42,0.,5.14351655641888E-17));
#7997=CARTESIAN_POINT('',(-0.42,0.,5.14351655641888E-17));
#7998=CARTESIAN_POINT('Origin',(0.,0.,0.));
#7999=CARTESIAN_POINT('Origin',(0.,0.,0.));
#8000=CARTESIAN_POINT('',(-0.8,0.16,9.79717439317883E-17));
#8001=CARTESIAN_POINT('Origin',(0.,0.16,0.));
#8002=CARTESIAN_POINT('',(-0.8,0.,9.79717439317883E-17));
#8003=CARTESIAN_POINT('',(-0.8,0.,9.79717439317883E-17));
#8004=CARTESIAN_POINT('Origin',(0.,0.,0.));
#8005=CARTESIAN_POINT('Origin',(0.,0.16,0.));
#8006=CARTESIAN_POINT('Origin',(0.,0.,0.));
#8007=CARTESIAN_POINT('',(0.,0.,0.));
#8008=CARTESIAN_POINT('Origin',(0.173205080756888,-0.8,-0.3));
#8009=CARTESIAN_POINT('',(0.346410161513775,-0.8,0.));
#8010=CARTESIAN_POINT('',(0.173205080756888,-0.8,-0.3));
#8011=CARTESIAN_POINT('',(0.346410161513775,-0.8,0.));
#8012=CARTESIAN_POINT('',(0.173205080756888,-1.28,-0.3));
#8013=CARTESIAN_POINT('',(0.173205080756888,-0.8,-0.3));
#8014=CARTESIAN_POINT('',(0.346410161513775,-1.28,0.));
#8015=CARTESIAN_POINT('',(0.346410161513775,-1.28,0.));
#8016=CARTESIAN_POINT('',(0.346410161513775,-0.8,0.));
#8017=CARTESIAN_POINT('Origin',(-0.173205080756888,-0.8,-0.3));
#8018=CARTESIAN_POINT('',(-0.173205080756888,-0.8,-0.3));
#8019=CARTESIAN_POINT('',(0.173205080756888,-0.8,-0.3));
#8020=CARTESIAN_POINT('',(-0.173205080756888,-1.28,-0.3));
#8021=CARTESIAN_POINT('',(-0.173205080756888,-0.8,-0.3));
#8022=CARTESIAN_POINT('',(0.173205080756888,-1.28,-0.3));
#8023=CARTESIAN_POINT('Origin',(-0.346410161513775,-0.8,-5.55111512312578E-17));
#8024=CARTESIAN_POINT('',(-0.346410161513775,-0.8,-4.24230095489963E-17));
#8025=CARTESIAN_POINT('',(-0.173205080756888,-0.8,-0.3));
#8026=CARTESIAN_POINT('',(-0.346410161513775,-1.28,-5.55111512312578E-17));
#8027=CARTESIAN_POINT('',(-0.346410161513775,-0.8,-4.24230095489963E-17));
#8028=CARTESIAN_POINT('',(-0.173205080756888,-1.28,-0.3));
#8029=CARTESIAN_POINT('Origin',(-0.173205080756888,-0.8,0.3));
#8030=CARTESIAN_POINT('',(-0.173205080756888,-0.8,0.3));
#8031=CARTESIAN_POINT('',(-0.346410161513775,-0.8,-4.24230095489963E-17));
#8032=CARTESIAN_POINT('',(-0.173205080756888,-1.28,0.3));
#8033=CARTESIAN_POINT('',(-0.173205080756888,-0.8,0.3));
#8034=CARTESIAN_POINT('',(-0.346410161513775,-1.28,-4.24230095489963E-17));
#8035=CARTESIAN_POINT('Origin',(0.173205080756888,-0.8,0.3));
#8036=CARTESIAN_POINT('',(0.173205080756888,-0.8,0.3));
#8037=CARTESIAN_POINT('',(-0.173205080756888,-0.8,0.3));
#8038=CARTESIAN_POINT('',(0.173205080756888,-1.28,0.3));
#8039=CARTESIAN_POINT('',(0.173205080756888,-0.8,0.3));
#8040=CARTESIAN_POINT('',(-0.173205080756888,-1.28,0.3));
#8041=CARTESIAN_POINT('Origin',(0.346410161513775,-0.8,0.));
#8042=CARTESIAN_POINT('',(0.173205080756888,-0.8,0.3));
#8043=CARTESIAN_POINT('',(0.173205080756888,-1.28,0.3));
#8044=CARTESIAN_POINT('Origin',(0.,-0.8,-5.55111512312578E-17));
#8045=CARTESIAN_POINT('Origin',(0.,-1.28,-5.55111512312578E-17));
#8046=CARTESIAN_POINT('Origin',(0.,-2.5,0.));
#8047=CARTESIAN_POINT('',(-0.3933,-2.5,4.81653586104654E-17));
#8048=CARTESIAN_POINT('Origin',(0.,-2.5,0.));
#8049=CARTESIAN_POINT('Origin',(0.6,0.8,0.));
#8050=CARTESIAN_POINT('',(-0.6,0.8,-7.34788079488412E-17));
#8051=CARTESIAN_POINT('Origin',(0.,0.8,0.));
#8052=CARTESIAN_POINT('Origin',(0.,0.775,0.));
#8053=CARTESIAN_POINT('',(-0.65,0.75,-7.9602041944578E-17));
#8054=CARTESIAN_POINT('Origin',(0.,0.75,0.));
#8055=CARTESIAN_POINT('',(-0.625,0.775,-7.65404249467096E-17));
#8056=CARTESIAN_POINT('Origin',(0.,0.39,0.));
#8057=CARTESIAN_POINT('',(-0.65,0.0299999999999998,-7.9602041944578E-17));
#8058=CARTESIAN_POINT('Origin',(0.,0.0299999999999998,0.));
#8059=CARTESIAN_POINT('',(-0.65,0.39,-7.9602041944578E-17));
#8060=CARTESIAN_POINT('Origin',(0.,0.0150000000000001,0.));
#8061=CARTESIAN_POINT('',(-0.62,5.89805981832114E-17,-7.59281015471359E-17));
#8062=CARTESIAN_POINT('Origin',(0.,0.,0.));
#8063=CARTESIAN_POINT('',(-0.635,0.0150000000000001,-7.77650717458569E-17));
#8064=CARTESIAN_POINT('Origin',(0.42,0.,0.));
#8065=CARTESIAN_POINT('',(-0.42,-3.46944695195361E-18,-5.14351655641888E-17));
#8066=CARTESIAN_POINT('Origin',(0.,0.,0.));
#8067=CARTESIAN_POINT('Origin',(0.,-0.02,0.));
#8068=CARTESIAN_POINT('',(-0.3933,-0.0534000000000001,4.81653586104654E-17));
#8069=CARTESIAN_POINT('Origin',(0.,-0.0534000000000001,0.));
#8070=CARTESIAN_POINT('',(-0.41,-0.02,-5.02105187650415E-17));
#8071=CARTESIAN_POINT('Origin',(0.,-1.48,0.));
#8072=CARTESIAN_POINT('',(-0.3933,-1.48,-4.81653586104654E-17));
#8073=CARTESIAN_POINT('',(0.,0.,0.));
#8074=CARTESIAN_POINT('',(0.,0.,0.));
#8075=CARTESIAN_POINT('Origin',(0.,-4.6,6.53));
#8076=CARTESIAN_POINT('',(-0.21,-4.5,6.53));
#8077=CARTESIAN_POINT('Origin',(0.,-4.5,6.53));
#8078=CARTESIAN_POINT('',(-0.21,-2.5,6.53));
#8079=CARTESIAN_POINT('',(-0.21,-4.6,6.53));
#8080=CARTESIAN_POINT('Origin',(0.,-2.5,6.53));
#8081=CARTESIAN_POINT('Origin',(0.,-2.5,6.53));
#8082=CARTESIAN_POINT('Origin',(-0.3,7.2,5.43));
#8083=CARTESIAN_POINT('',(-0.3,9.2,5.57606079858305));
#8084=CARTESIAN_POINT('',(-0.3,7.2,5.57606079858305));
#8085=CARTESIAN_POINT('',(-0.3,-4.5,5.57606079858305));
#8086=CARTESIAN_POINT('',(-0.3,9.2,5.88));
#8087=CARTESIAN_POINT('',(-0.3,9.2,5.88));
#8088=CARTESIAN_POINT('',(-0.3,7.2,5.88));
#8089=CARTESIAN_POINT('',(-0.3,7.2,5.88));
#8090=CARTESIAN_POINT('',(-0.3,7.2,5.88));
#8091=CARTESIAN_POINT('Origin',(0.,7.2,5.655));
#8092=CARTESIAN_POINT('',(0.3,7.2,5.57606079858305));
#8093=CARTESIAN_POINT('Origin',(0.,7.2,6.53));
#8094=CARTESIAN_POINT('',(0.3,7.2,5.88));
#8095=CARTESIAN_POINT('',(0.3,7.2,5.88));
#8096=CARTESIAN_POINT('',(0.3,7.2,5.43));
#8097=CARTESIAN_POINT('Origin',(0.3,7.2,5.88));
#8098=CARTESIAN_POINT('',(0.3,9.2,5.57606079858305));
#8099=CARTESIAN_POINT('',(0.3,-4.5,5.57606079858305));
#8100=CARTESIAN_POINT('',(0.3,9.2,5.88));
#8101=CARTESIAN_POINT('',(0.3,7.2,5.88));
#8102=CARTESIAN_POINT('',(0.3,9.2,5.43));
#8103=CARTESIAN_POINT('Origin',(-0.3,7.2,5.88));
#8104=CARTESIAN_POINT('',(0.3,9.2,5.88));
#8105=CARTESIAN_POINT('Origin',(0.,9.2,5.655));
#8106=CARTESIAN_POINT('Origin',(0.,9.2,6.53));
#8107=CARTESIAN_POINT('Origin',(0.,-4.5,6.53));
#8108=CARTESIAN_POINT('',(-1.,10.,6.53));
#8109=CARTESIAN_POINT('Origin',(0.,10.,6.53));
#8110=CARTESIAN_POINT('',(-1.,-4.5,6.53));
#8111=CARTESIAN_POINT('',(-1.,-4.5,6.53));
#8112=CARTESIAN_POINT('Origin',(0.,-4.5,6.53));
#8113=CARTESIAN_POINT('Origin',(0.,10.,6.53));
#8114=CARTESIAN_POINT('Origin',(0.,-4.5,6.53));
#8115=CARTESIAN_POINT('',(0.,0.,0.));
#8116=CARTESIAN_POINT('Origin',(-2.12132034355964,9.3,4.40867965644036));
#8117=CARTESIAN_POINT('',(-2.45132034355964,9.4,4.40867965644036));
#8118=CARTESIAN_POINT('Origin',(-2.12132034355964,9.4,4.40867965644036));
#8119=CARTESIAN_POINT('',(-2.45132034355964,10.,4.40867965644036));
#8120=CARTESIAN_POINT('',(-2.45132034355964,9.3,4.40867965644036));
#8121=CARTESIAN_POINT('Origin',(-2.12132034355964,10.,4.40867965644036));
#8122=CARTESIAN_POINT('Origin',(-2.12132034355964,9.3,8.65132034355964));
#8123=CARTESIAN_POINT('',(-2.45132034355964,9.4,8.65132034355964));
#8124=CARTESIAN_POINT('Origin',(-2.12132034355964,9.4,8.65132034355964));
#8125=CARTESIAN_POINT('',(-2.45132034355964,10.,8.65132034355964));
#8126=CARTESIAN_POINT('',(-2.45132034355964,9.3,8.65132034355964));
#8127=CARTESIAN_POINT('Origin',(-2.12132034355964,10.,8.65132034355964));
#8128=CARTESIAN_POINT('Origin',(2.12132034355964,9.3,8.65132034355964));
#8129=CARTESIAN_POINT('',(1.79132034355964,9.4,8.65132034355964));
#8130=CARTESIAN_POINT('Origin',(2.12132034355964,9.4,8.65132034355964));
#8131=CARTESIAN_POINT('',(1.79132034355964,10.,8.65132034355964));
#8132=CARTESIAN_POINT('',(1.79132034355964,9.3,8.65132034355964));
#8133=CARTESIAN_POINT('Origin',(2.12132034355964,10.,8.65132034355964));
#8134=CARTESIAN_POINT('Origin',(2.12132034355964,9.3,4.40867965644036));
#8135=CARTESIAN_POINT('',(1.79132034355964,9.4,4.40867965644036));
#8136=CARTESIAN_POINT('Origin',(2.12132034355964,9.4,4.40867965644036));
#8137=CARTESIAN_POINT('',(1.79132034355964,10.,4.40867965644036));
#8138=CARTESIAN_POINT('',(1.79132034355964,9.3,4.40867965644036));
#8139=CARTESIAN_POINT('Origin',(2.12132034355964,10.,4.40867965644036));
#8140=CARTESIAN_POINT('Origin',(0.,8.2,7.52));
#8141=CARTESIAN_POINT('',(0.141067359796651,8.04443650813895,7.52));
#8142=CARTESIAN_POINT('',(0.141067359796651,8.35556349186105,7.52));
#8143=CARTESIAN_POINT('',(0.141067359796651,7.,7.52));
#8144=CARTESIAN_POINT('Origin',(0.,8.2,7.52));
#8145=CARTESIAN_POINT('Origin',(0.,8.2,7.52));
#8146=CARTESIAN_POINT('',(-0.141067359796651,8.04443650813895,7.52));
#8147=CARTESIAN_POINT('Ctrl Pts',(-0.141067359796651,8.04443650813895,7.52));
#8148=CARTESIAN_POINT('Ctrl Pts',(-0.123818356698219,8.0287948476368,7.52245784982447));
#8149=CARTESIAN_POINT('Ctrl Pts',(-0.102998643109696,8.01537595666898,7.52493819304946));
#8150=CARTESIAN_POINT('Ctrl Pts',(-0.0546141143983529,7.99530253627557,
7.52884449237241));
#8151=CARTESIAN_POINT('Ctrl Pts',(-0.0264520736824499,7.99,7.53));
#8152=CARTESIAN_POINT('Ctrl Pts',(0.0264520736824498,7.99,7.53));
#8153=CARTESIAN_POINT('Ctrl Pts',(0.0546141143983527,7.99530253627557,7.52884449237241));
#8154=CARTESIAN_POINT('Ctrl Pts',(0.102998643109696,8.01537595666898,7.52493819304946));
#8155=CARTESIAN_POINT('Ctrl Pts',(0.123818356698219,8.0287948476368,7.52245784982447));
#8156=CARTESIAN_POINT('Ctrl Pts',(0.141067359796651,8.04443650813895,7.52));
#8157=CARTESIAN_POINT('',(-0.21,8.2,7.52));
#8158=CARTESIAN_POINT('Origin',(0.,8.2,7.52));
#8159=CARTESIAN_POINT('',(-0.21,8.2,8.21697954937219));
#8160=CARTESIAN_POINT('',(-0.21,8.2,7.52));
#8161=CARTESIAN_POINT('',(0.21,8.2,8.21697954937219));
#8162=CARTESIAN_POINT('Ctrl Pts',(0.21,8.2,8.21697954937219));
#8163=CARTESIAN_POINT('Ctrl Pts',(0.21,8.17360286013118,8.21697954937219));
#8164=CARTESIAN_POINT('Ctrl Pts',(0.204718998643499,8.14546483574125,8.21766304765575));
#8165=CARTESIAN_POINT('Ctrl Pts',(0.183279390356407,8.09373326708872,8.22012576310987));
#8166=CARTESIAN_POINT('Ctrl Pts',(0.167122246533942,8.07013739843559,8.22186875774124));
#8167=CARTESIAN_POINT('Ctrl Pts',(0.129862749952602,8.03287790185425,8.22513580556568));
#8168=CARTESIAN_POINT('Ctrl Pts',(0.106266816759542,8.0167206417943,8.22687297932906));
#8169=CARTESIAN_POINT('Ctrl Pts',(0.0545350296960238,7.99528094818772,8.22932235754078));
#8170=CARTESIAN_POINT('Ctrl Pts',(0.026396929613248,7.99,8.23));
#8171=CARTESIAN_POINT('Ctrl Pts',(-0.026396929613248,7.99,8.23));
#8172=CARTESIAN_POINT('Ctrl Pts',(-0.0545350296960238,7.99528094818772,
8.22932235754078));
#8173=CARTESIAN_POINT('Ctrl Pts',(-0.106266816759542,8.0167206417943,8.22687297932906));
#8174=CARTESIAN_POINT('Ctrl Pts',(-0.129862749952602,8.03287790185425,8.22513580556568));
#8175=CARTESIAN_POINT('Ctrl Pts',(-0.167122246533942,8.07013739843559,8.22186875774124));
#8176=CARTESIAN_POINT('Ctrl Pts',(-0.183279390356407,8.09373326708872,8.22012576310987));
#8177=CARTESIAN_POINT('Ctrl Pts',(-0.204718998643499,8.14546483574125,8.21766304765575));
#8178=CARTESIAN_POINT('Ctrl Pts',(-0.21,8.17360286013118,8.21697954937219));
#8179=CARTESIAN_POINT('Ctrl Pts',(-0.21,8.2,8.21697954937219));
#8180=CARTESIAN_POINT('Ctrl Pts',(-0.21,8.2,8.21697954937219));
#8181=CARTESIAN_POINT('Ctrl Pts',(-0.21,8.22639713986882,8.21697954937219));
#8182=CARTESIAN_POINT('Ctrl Pts',(-0.204718998643499,8.25453516425875,8.21766304765575));
#8183=CARTESIAN_POINT('Ctrl Pts',(-0.183279390356407,8.30626673291128,8.22012576310987));
#8184=CARTESIAN_POINT('Ctrl Pts',(-0.167122246533942,8.32986260156441,8.22186875774124));
#8185=CARTESIAN_POINT('Ctrl Pts',(-0.129862749952602,8.36712209814575,8.22513580556568));
#8186=CARTESIAN_POINT('Ctrl Pts',(-0.106266816759542,8.3832793582057,8.22687297932906));
#8187=CARTESIAN_POINT('Ctrl Pts',(-0.0545350296960238,8.40471905181228,
8.22932235754078));
#8188=CARTESIAN_POINT('Ctrl Pts',(-0.0263969296132481,8.41,8.23));
#8189=CARTESIAN_POINT('Ctrl Pts',(0.026396929613248,8.41,8.23));
#8190=CARTESIAN_POINT('Ctrl Pts',(0.0545350296960237,8.40471905181228,8.22932235754078));
#8191=CARTESIAN_POINT('Ctrl Pts',(0.106266816759542,8.3832793582057,8.22687297932906));
#8192=CARTESIAN_POINT('Ctrl Pts',(0.129862749952602,8.36712209814575,8.22513580556568));
#8193=CARTESIAN_POINT('Ctrl Pts',(0.167122246533941,8.32986260156441,8.22186875774124));
#8194=CARTESIAN_POINT('Ctrl Pts',(0.183279390356407,8.30626673291128,8.22012576310987));
#8195=CARTESIAN_POINT('Ctrl Pts',(0.204718998643499,8.25453516425875,8.21766304765575));
#8196=CARTESIAN_POINT('Ctrl Pts',(0.21,8.22639713986882,8.21697954937219));
#8197=CARTESIAN_POINT('Ctrl Pts',(0.21,8.2,8.21697954937219));
#8198=CARTESIAN_POINT('',(-0.141067359796651,8.35556349186105,7.52));
#8199=CARTESIAN_POINT('Origin',(0.,8.2,7.52));
#8200=CARTESIAN_POINT('Ctrl Pts',(0.14106735979665,8.35556349186105,7.52));
#8201=CARTESIAN_POINT('Ctrl Pts',(0.123818356698217,8.3712051523632,7.52245784982447));
#8202=CARTESIAN_POINT('Ctrl Pts',(0.102998643109696,8.38462404333102,7.52493819304946));
#8203=CARTESIAN_POINT('Ctrl Pts',(0.0546141143983528,8.40469746372443,7.52884449237241));
#8204=CARTESIAN_POINT('Ctrl Pts',(0.0264520736824499,8.41,7.53));
#8205=CARTESIAN_POINT('Ctrl Pts',(-0.0264520736824498,8.41,7.53));
#8206=CARTESIAN_POINT('Ctrl Pts',(-0.0546141143983528,8.40469746372443,
7.52884449237241));
#8207=CARTESIAN_POINT('Ctrl Pts',(-0.102998643109695,8.38462404333102,7.52493819304946));
#8208=CARTESIAN_POINT('Ctrl Pts',(-0.123818356698218,8.3712051523632,7.52245784982447));
#8209=CARTESIAN_POINT('Ctrl Pts',(-0.14106735979665,8.35556349186105,7.52));
#8210=CARTESIAN_POINT('Origin',(0.,8.2,7.52));
#8211=CARTESIAN_POINT('',(-0.141067359796651,7.,7.52));
#8212=CARTESIAN_POINT('Origin',(-0.3,6.9,5.25));
#8213=CARTESIAN_POINT('',(-0.3,7.,5.25));
#8214=CARTESIAN_POINT('',(-0.3,7.,5.57606079858305));
#8215=CARTESIAN_POINT('',(-0.3,7.,5.89));
#8216=CARTESIAN_POINT('',(-0.3,9.8,5.25));
#8217=CARTESIAN_POINT('',(-0.3,6.9,5.25));
#8218=CARTESIAN_POINT('',(-0.3,9.8,5.57606079858305));
#8219=CARTESIAN_POINT('',(-0.3,9.8,5.89));
#8220=CARTESIAN_POINT('',(-0.3,7.,5.57606079858305));
#8221=CARTESIAN_POINT('Origin',(0.3,6.9,5.25));
#8222=CARTESIAN_POINT('',(0.3,7.,5.25));
#8223=CARTESIAN_POINT('',(0.15,7.,5.25));
#8224=CARTESIAN_POINT('',(0.3,9.8,5.25));
#8225=CARTESIAN_POINT('',(0.3,6.9,5.25));
#8226=CARTESIAN_POINT('',(0.15,9.8,5.25));
#8227=CARTESIAN_POINT('Origin',(0.3,6.9,6.53));
#8228=CARTESIAN_POINT('',(0.3,7.,5.57606079858305));
#8229=CARTESIAN_POINT('',(0.3,7.,6.53));
#8230=CARTESIAN_POINT('',(0.3,9.8,5.57606079858305));
#8231=CARTESIAN_POINT('',(0.3,7.,5.57606079858305));
#8232=CARTESIAN_POINT('',(0.3,9.8,6.53));
#8233=CARTESIAN_POINT('Origin',(0.,7.,6.53));
#8234=CARTESIAN_POINT('',(-1.7,7.,6.53));
#8235=CARTESIAN_POINT('Origin',(0.,7.,6.53));
#8236=CARTESIAN_POINT('Origin',(0.,7.,6.53));
#8237=CARTESIAN_POINT('Origin',(0.,9.8,6.53));
#8238=CARTESIAN_POINT('',(-2.,9.8,6.53));
#8239=CARTESIAN_POINT('Origin',(0.,9.8,6.53));
#8240=CARTESIAN_POINT('',(-2.,10.,6.53));
#8241=CARTESIAN_POINT('',(-2.,9.8,6.53));
#8242=CARTESIAN_POINT('Origin',(0.,10.,6.53));
#8243=CARTESIAN_POINT('Origin',(0.,9.8,6.53));
#8244=CARTESIAN_POINT('Origin',(0.,9.8,6.53));
#8245=CARTESIAN_POINT('Origin',(0.,9.4,6.53));
#8246=CARTESIAN_POINT('',(-4.,9.4,6.53));
#8247=CARTESIAN_POINT('Origin',(0.,9.4,6.53));
#8248=CARTESIAN_POINT('',(-1.7,9.4,6.53));
#8249=CARTESIAN_POINT('Origin',(0.,9.4,6.53));
#8250=CARTESIAN_POINT('Origin',(0.,9.4,6.53));
#8251=CARTESIAN_POINT('',(-4.,10.,6.53));
#8252=CARTESIAN_POINT('Origin',(0.,10.,6.53));
#8253=CARTESIAN_POINT('',(-4.,9.4,6.53));
#8254=CARTESIAN_POINT('Origin',(0.,7.,6.53));
#8255=CARTESIAN_POINT('Origin',(0.,7.,6.53));
#8256=CARTESIAN_POINT('',(-1.7,7.,6.53));
#8257=CARTESIAN_POINT('Origin',(0.,10.,6.53));
#8258=CARTESIAN_POINT('',(0.,0.,0.));
#8259=CARTESIAN_POINT('Origin',(0.,-4.7,6.53));
#8260=CARTESIAN_POINT('',(-0.275,-4.5,6.53));
#8261=CARTESIAN_POINT('Origin',(0.,-4.5,6.53));
#8262=CARTESIAN_POINT('',(-0.275,-4.7,6.53));
#8263=CARTESIAN_POINT('',(-0.275,-4.7,6.53));
#8264=CARTESIAN_POINT('Origin',(0.,-4.7,6.53));
#8265=CARTESIAN_POINT('Origin',(0.,-4.7,6.53));
#8266=CARTESIAN_POINT('',(-1.1,-4.5,6.53));
#8267=CARTESIAN_POINT('Origin',(0.,-4.5,6.53));
#8268=CARTESIAN_POINT('',(-1.1,-4.7,6.53));
#8269=CARTESIAN_POINT('',(-1.1,-4.7,6.53));
#8270=CARTESIAN_POINT('Origin',(0.,-4.7,6.53));
#8271=CARTESIAN_POINT('Origin',(0.,-4.5,6.53));
#8272=CARTESIAN_POINT('Origin',(0.,-4.7,6.53));
#8273=CARTESIAN_POINT('',(0.,0.,0.));
#8274=CARTESIAN_POINT('Origin',(0.,22.5,6.53));
#8275=CARTESIAN_POINT('',(-0.21,22.5,6.53));
#8276=CARTESIAN_POINT('Origin',(0.,22.5,6.53));
#8277=CARTESIAN_POINT('',(-0.21,24.5,6.53));
#8278=CARTESIAN_POINT('',(-0.21,22.5,6.53));
#8279=CARTESIAN_POINT('Origin',(0.,24.5,6.53));
#8280=CARTESIAN_POINT('Origin',(0.,22.5,6.53));
#8281=CARTESIAN_POINT('Origin',(-0.3,10.8,5.43));
#8282=CARTESIAN_POINT('',(-0.3,12.8,5.57606079858305));
#8283=CARTESIAN_POINT('',(-0.3,10.8,5.57606079858305));
#8284=CARTESIAN_POINT('',(-0.3,10.,5.57606079858305));
#8285=CARTESIAN_POINT('',(-0.3,12.8,5.88));
#8286=CARTESIAN_POINT('',(-0.3,12.8,5.88));
#8287=CARTESIAN_POINT('',(-0.3,10.8,5.88));
#8288=CARTESIAN_POINT('',(-0.3,10.8,5.88));
#8289=CARTESIAN_POINT('',(-0.3,10.8,5.88));
#8290=CARTESIAN_POINT('Origin',(0.,10.8,5.655));
#8291=CARTESIAN_POINT('',(0.3,10.8,5.57606079858305));
#8292=CARTESIAN_POINT('Origin',(0.,10.8,6.53));
#8293=CARTESIAN_POINT('',(0.3,10.8,5.88));
#8294=CARTESIAN_POINT('',(0.3,10.8,5.88));
#8295=CARTESIAN_POINT('',(0.3,10.8,5.43));
#8296=CARTESIAN_POINT('Origin',(0.3,10.8,5.88));
#8297=CARTESIAN_POINT('',(0.3,12.8,5.57606079858305));
#8298=CARTESIAN_POINT('',(0.3,10.,5.57606079858305));
#8299=CARTESIAN_POINT('',(0.3,12.8,5.88));
#8300=CARTESIAN_POINT('',(0.3,10.8,5.88));
#8301=CARTESIAN_POINT('',(0.3,12.8,5.43));
#8302=CARTESIAN_POINT('Origin',(-0.3,10.8,5.88));
#8303=CARTESIAN_POINT('',(0.3,12.8,5.88));
#8304=CARTESIAN_POINT('Origin',(0.,12.8,5.655));
#8305=CARTESIAN_POINT('Origin',(0.,12.8,6.53));
#8306=CARTESIAN_POINT('Origin',(0.,10.,6.53));
#8307=CARTESIAN_POINT('',(-1.,24.5,6.53));
#8308=CARTESIAN_POINT('Origin',(0.,24.5,6.53));
#8309=CARTESIAN_POINT('',(-1.,10.,6.53));
#8310=CARTESIAN_POINT('',(-1.,10.,6.53));
#8311=CARTESIAN_POINT('Origin',(0.,10.,6.53));
#8312=CARTESIAN_POINT('Origin',(0.,24.5,6.53));
#8313=CARTESIAN_POINT('Origin',(0.,10.,6.53));
#8314=CARTESIAN_POINT('',(0.,0.,0.));
#8315=CARTESIAN_POINT('Origin',(-2.12132034355964,9.3,4.40867965644036));
#8316=CARTESIAN_POINT('',(-2.45132034355964,10.,4.40867965644036));
#8317=CARTESIAN_POINT('Origin',(-2.12132034355964,10.,4.40867965644036));
#8318=CARTESIAN_POINT('',(-2.45132034355964,10.6,4.40867965644036));
#8319=CARTESIAN_POINT('',(-2.45132034355964,9.3,4.40867965644036));
#8320=CARTESIAN_POINT('Origin',(-2.12132034355964,10.6,4.40867965644036));
#8321=CARTESIAN_POINT('Origin',(-2.12132034355964,9.3,8.65132034355964));
#8322=CARTESIAN_POINT('',(-2.45132034355964,10.,8.65132034355964));
#8323=CARTESIAN_POINT('Origin',(-2.12132034355964,10.,8.65132034355964));
#8324=CARTESIAN_POINT('',(-2.45132034355964,10.6,8.65132034355964));
#8325=CARTESIAN_POINT('',(-2.45132034355964,9.3,8.65132034355964));
#8326=CARTESIAN_POINT('Origin',(-2.12132034355964,10.6,8.65132034355964));
#8327=CARTESIAN_POINT('Origin',(2.12132034355964,9.3,8.65132034355964));
#8328=CARTESIAN_POINT('',(1.79132034355964,10.,8.65132034355964));
#8329=CARTESIAN_POINT('Origin',(2.12132034355964,10.,8.65132034355964));
#8330=CARTESIAN_POINT('',(1.79132034355964,10.6,8.65132034355964));
#8331=CARTESIAN_POINT('',(1.79132034355964,9.3,8.65132034355964));
#8332=CARTESIAN_POINT('Origin',(2.12132034355964,10.6,8.65132034355964));
#8333=CARTESIAN_POINT('Origin',(2.12132034355964,9.3,4.40867965644036));
#8334=CARTESIAN_POINT('',(1.79132034355964,10.,4.40867965644036));
#8335=CARTESIAN_POINT('Origin',(2.12132034355964,10.,4.40867965644036));
#8336=CARTESIAN_POINT('',(1.79132034355964,10.6,4.40867965644036));
#8337=CARTESIAN_POINT('',(1.79132034355964,9.3,4.40867965644036));
#8338=CARTESIAN_POINT('Origin',(2.12132034355964,10.6,4.40867965644036));
#8339=CARTESIAN_POINT('Origin',(0.,11.8,7.52));
#8340=CARTESIAN_POINT('',(0.141067359796651,11.644436508139,7.52));
#8341=CARTESIAN_POINT('',(0.141067359796651,11.955563491861,7.52));
#8342=CARTESIAN_POINT('',(0.141067359796651,10.,7.52));
#8343=CARTESIAN_POINT('Origin',(0.,11.8,7.52));
#8344=CARTESIAN_POINT('Origin',(0.,11.8,7.52));
#8345=CARTESIAN_POINT('',(-0.141067359796651,11.644436508139,7.52));
#8346=CARTESIAN_POINT('Ctrl Pts',(-0.141067359796652,11.644436508139,7.52));
#8347=CARTESIAN_POINT('Ctrl Pts',(-0.12381835669822,11.6287948476368,7.52245784982447));
#8348=CARTESIAN_POINT('Ctrl Pts',(-0.102998643109696,11.615375956669,7.52493819304946));
#8349=CARTESIAN_POINT('Ctrl Pts',(-0.0546141143983528,11.5953025362756,
7.52884449237241));
#8350=CARTESIAN_POINT('Ctrl Pts',(-0.0264520736824499,11.59,7.53));
#8351=CARTESIAN_POINT('Ctrl Pts',(0.0264520736824499,11.59,7.53));
#8352=CARTESIAN_POINT('Ctrl Pts',(0.054614114398353,11.5953025362756,7.52884449237241));
#8353=CARTESIAN_POINT('Ctrl Pts',(0.102998643109697,11.615375956669,7.52493819304946));
#8354=CARTESIAN_POINT('Ctrl Pts',(0.123818356698218,11.6287948476368,7.52245784982447));
#8355=CARTESIAN_POINT('Ctrl Pts',(0.141067359796651,11.644436508139,7.52));
#8356=CARTESIAN_POINT('',(-0.21,11.8,7.52));
#8357=CARTESIAN_POINT('Origin',(0.,11.8,7.52));
#8358=CARTESIAN_POINT('',(-0.21,11.8,8.21697954937219));
#8359=CARTESIAN_POINT('',(-0.21,11.8,7.52));
#8360=CARTESIAN_POINT('',(0.21,11.8,8.21697954937219));
#8361=CARTESIAN_POINT('Ctrl Pts',(0.21,11.8,8.21697954937219));
#8362=CARTESIAN_POINT('Ctrl Pts',(0.21,11.7736028601312,8.21697954937219));
#8363=CARTESIAN_POINT('Ctrl Pts',(0.204718998643499,11.7454648357413,8.21766304765575));
#8364=CARTESIAN_POINT('Ctrl Pts',(0.183279390356407,11.6937332670887,8.22012576310987));
#8365=CARTESIAN_POINT('Ctrl Pts',(0.167122246533942,11.6701373984356,8.22186875774124));
#8366=CARTESIAN_POINT('Ctrl Pts',(0.129862749952602,11.6328779018543,8.22513580556568));
#8367=CARTESIAN_POINT('Ctrl Pts',(0.106266816759542,11.6167206417943,8.22687297932906));
#8368=CARTESIAN_POINT('Ctrl Pts',(0.0545350296960238,11.5952809481877,8.22932235754078));
#8369=CARTESIAN_POINT('Ctrl Pts',(0.0263969296132481,11.59,8.23));
#8370=CARTESIAN_POINT('Ctrl Pts',(-0.026396929613248,11.59,8.23));
#8371=CARTESIAN_POINT('Ctrl Pts',(-0.0545350296960238,11.5952809481877,
8.22932235754078));
#8372=CARTESIAN_POINT('Ctrl Pts',(-0.106266816759542,11.6167206417943,8.22687297932906));
#8373=CARTESIAN_POINT('Ctrl Pts',(-0.129862749952602,11.6328779018543,8.22513580556568));
#8374=CARTESIAN_POINT('Ctrl Pts',(-0.167122246533941,11.6701373984356,8.22186875774124));
#8375=CARTESIAN_POINT('Ctrl Pts',(-0.183279390356407,11.6937332670887,8.22012576310987));
#8376=CARTESIAN_POINT('Ctrl Pts',(-0.204718998643499,11.7454648357413,8.21766304765575));
#8377=CARTESIAN_POINT('Ctrl Pts',(-0.21,11.7736028601312,8.21697954937219));
#8378=CARTESIAN_POINT('Ctrl Pts',(-0.21,11.8,8.21697954937219));
#8379=CARTESIAN_POINT('Ctrl Pts',(-0.21,11.8,8.21697954937219));
#8380=CARTESIAN_POINT('Ctrl Pts',(-0.21,11.8263971398688,8.21697954937219));
#8381=CARTESIAN_POINT('Ctrl Pts',(-0.204718998643499,11.8545351642587,8.21766304765575));
#8382=CARTESIAN_POINT('Ctrl Pts',(-0.183279390356407,11.9062667329113,8.22012576310987));
#8383=CARTESIAN_POINT('Ctrl Pts',(-0.167122246533942,11.9298626015644,8.22186875774124));
#8384=CARTESIAN_POINT('Ctrl Pts',(-0.129862749952602,11.9671220981457,8.22513580556568));
#8385=CARTESIAN_POINT('Ctrl Pts',(-0.106266816759542,11.9832793582057,8.22687297932906));
#8386=CARTESIAN_POINT('Ctrl Pts',(-0.0545350296960238,12.0047190518123,
8.22932235754078));
#8387=CARTESIAN_POINT('Ctrl Pts',(-0.0263969296132481,12.01,8.23));
#8388=CARTESIAN_POINT('Ctrl Pts',(0.026396929613248,12.01,8.23));
#8389=CARTESIAN_POINT('Ctrl Pts',(0.0545350296960238,12.0047190518123,8.22932235754078));
#8390=CARTESIAN_POINT('Ctrl Pts',(0.106266816759542,11.9832793582057,8.22687297932906));
#8391=CARTESIAN_POINT('Ctrl Pts',(0.129862749952602,11.9671220981457,8.22513580556568));
#8392=CARTESIAN_POINT('Ctrl Pts',(0.167122246533941,11.9298626015644,8.22186875774124));
#8393=CARTESIAN_POINT('Ctrl Pts',(0.183279390356408,11.9062667329113,8.22012576310987));
#8394=CARTESIAN_POINT('Ctrl Pts',(0.204718998643499,11.8545351642587,8.21766304765575));
#8395=CARTESIAN_POINT('Ctrl Pts',(0.21,11.8263971398688,8.21697954937219));
#8396=CARTESIAN_POINT('Ctrl Pts',(0.21,11.8,8.21697954937219));
#8397=CARTESIAN_POINT('',(-0.141067359796651,11.955563491861,7.52));
#8398=CARTESIAN_POINT('Origin',(0.,11.8,7.52));
#8399=CARTESIAN_POINT('Ctrl Pts',(0.141067359796651,11.955563491861,7.52));
#8400=CARTESIAN_POINT('Ctrl Pts',(0.123818356698221,11.9712051523632,7.52245784982447));
#8401=CARTESIAN_POINT('Ctrl Pts',(0.102998643109695,11.984624043331,7.52493819304946));
#8402=CARTESIAN_POINT('Ctrl Pts',(0.0546141143983528,12.0046974637244,7.52884449237241));
#8403=CARTESIAN_POINT('Ctrl Pts',(0.0264520736824499,12.01,7.53));
#8404=CARTESIAN_POINT('Ctrl Pts',(-0.0264520736824498,12.01,7.53));
#8405=CARTESIAN_POINT('Ctrl Pts',(-0.0546141143983515,12.0046974637244,
7.52884449237241));
#8406=CARTESIAN_POINT('Ctrl Pts',(-0.102998643109696,11.984624043331,7.52493819304946));
#8407=CARTESIAN_POINT('Ctrl Pts',(-0.123818356698219,11.9712051523632,7.52245784982447));
#8408=CARTESIAN_POINT('Ctrl Pts',(-0.14106735979665,11.955563491861,7.52));
#8409=CARTESIAN_POINT('Origin',(0.,11.8,7.52));
#8410=CARTESIAN_POINT('',(-0.141067359796651,10.,7.52));
#8411=CARTESIAN_POINT('Origin',(0.3,9.9,6.53));
#8412=CARTESIAN_POINT('',(0.3,13.,5.25));
#8413=CARTESIAN_POINT('',(0.3,13.,5.57606079858305));
#8414=CARTESIAN_POINT('',(0.3,13.,6.53));
#8415=CARTESIAN_POINT('',(0.3,10.2,5.25));
#8416=CARTESIAN_POINT('',(0.3,9.9,5.25));
#8417=CARTESIAN_POINT('',(0.3,10.2,5.57606079858305));
#8418=CARTESIAN_POINT('',(0.3,10.2,6.53));
#8419=CARTESIAN_POINT('',(0.3,10.,5.57606079858305));
#8420=CARTESIAN_POINT('Origin',(-0.3,9.9,5.25));
#8421=CARTESIAN_POINT('',(-0.3,13.,5.57606079858305));
#8422=CARTESIAN_POINT('',(-0.3,13.,5.25));
#8423=CARTESIAN_POINT('',(-0.3,13.,5.89));
#8424=CARTESIAN_POINT('',(-0.3,10.2,5.57606079858305));
#8425=CARTESIAN_POINT('',(-0.3,10.,5.57606079858305));
#8426=CARTESIAN_POINT('',(-0.3,10.2,5.25));
#8427=CARTESIAN_POINT('',(-0.3,10.2,5.89));
#8428=CARTESIAN_POINT('',(-0.3,9.9,5.25));
#8429=CARTESIAN_POINT('Origin',(0.3,9.9,5.25));
#8430=CARTESIAN_POINT('',(0.15,13.,5.25));
#8431=CARTESIAN_POINT('',(0.15,10.2,5.25));
#8432=CARTESIAN_POINT('Origin',(0.,10.2,6.53));
#8433=CARTESIAN_POINT('',(-2.,10.2,6.53));
#8434=CARTESIAN_POINT('Origin',(0.,10.2,6.53));
#8435=CARTESIAN_POINT('Origin',(0.,10.2,6.53));
#8436=CARTESIAN_POINT('Origin',(0.,10.,6.53));
#8437=CARTESIAN_POINT('Origin',(0.,13.,6.53));
#8438=CARTESIAN_POINT('Origin',(0.,9.99,6.53));
#8439=CARTESIAN_POINT('',(-2.,10.,6.53));
#8440=CARTESIAN_POINT('Origin',(0.,10.,6.53));
#8441=CARTESIAN_POINT('',(-2.,9.99,6.53));
#8442=CARTESIAN_POINT('Origin',(0.,10.6,6.53));
#8443=CARTESIAN_POINT('',(-4.,10.6,6.53));
#8444=CARTESIAN_POINT('Origin',(0.,10.6,6.53));
#8445=CARTESIAN_POINT('',(-1.7,10.6,6.53));
#8446=CARTESIAN_POINT('Origin',(0.,10.6,6.53));
#8447=CARTESIAN_POINT('Origin',(0.,10.,6.53));
#8448=CARTESIAN_POINT('',(-4.,10.,6.53));
#8449=CARTESIAN_POINT('',(-4.,10.,6.53));
#8450=CARTESIAN_POINT('Origin',(0.,10.,6.53));
#8451=CARTESIAN_POINT('Origin',(0.,10.,6.53));
#8452=CARTESIAN_POINT('',(-1.7,13.,6.53));
#8453=CARTESIAN_POINT('Origin',(0.,13.,6.53));
#8454=CARTESIAN_POINT('',(-1.7,10.,6.53));
#8455=CARTESIAN_POINT('Origin',(0.,13.,6.53));
#8456=CARTESIAN_POINT('Origin',(0.,10.,6.53));
#8457=CARTESIAN_POINT('',(0.,0.,0.));
#8458=CARTESIAN_POINT('Origin',(0.,24.5,6.53));
#8459=CARTESIAN_POINT('',(-0.275,24.7,6.53));
#8460=CARTESIAN_POINT('Origin',(0.,24.7,6.53));
#8461=CARTESIAN_POINT('',(-0.275,24.5,6.53));
#8462=CARTESIAN_POINT('',(-0.275,24.5,6.53));
#8463=CARTESIAN_POINT('Origin',(0.,24.5,6.53));
#8464=CARTESIAN_POINT('Origin',(0.,24.5,6.53));
#8465=CARTESIAN_POINT('',(-1.1,24.7,6.53));
#8466=CARTESIAN_POINT('Origin',(0.,24.7,6.53));
#8467=CARTESIAN_POINT('',(-1.1,24.5,6.53));
#8468=CARTESIAN_POINT('',(-1.1,24.5,6.53));
#8469=CARTESIAN_POINT('Origin',(0.,24.5,6.53));
#8470=CARTESIAN_POINT('Origin',(0.,24.7,6.53));
#8471=CARTESIAN_POINT('Origin',(0.,24.5,6.53));
#8472=CARTESIAN_POINT('',(0.,0.,0.));
#8473=CARTESIAN_POINT('Origin',(0.,9.8,6.53));
#8474=CARTESIAN_POINT('',(-1.,10.2,6.53));
#8475=CARTESIAN_POINT('Origin',(0.,10.2,6.53));
#8476=CARTESIAN_POINT('',(-1.,9.8,6.53));
#8477=CARTESIAN_POINT('',(-1.,9.8,6.53));
#8478=CARTESIAN_POINT('Origin',(0.,9.8,6.53));
#8479=CARTESIAN_POINT('Origin',(0.,9.8,6.53));
#8480=CARTESIAN_POINT('',(-2.,10.2,6.53));
#8481=CARTESIAN_POINT('Origin',(0.,10.2,6.53));
#8482=CARTESIAN_POINT('',(-2.,9.8,6.53));
#8483=CARTESIAN_POINT('',(-2.,9.8,6.53));
#8484=CARTESIAN_POINT('Origin',(0.,9.8,6.53));
#8485=CARTESIAN_POINT('Origin',(0.,10.2,6.53));
#8486=CARTESIAN_POINT('Origin',(0.,9.8,6.53));
#8487=CARTESIAN_POINT('',(0.,0.,0.));
#8488=CARTESIAN_POINT('Origin',(0.,-1.25,7.52));
#8489=CARTESIAN_POINT('',(0.172988438920056,-1.36905880899792,7.52));
#8490=CARTESIAN_POINT('',(0.172988438920056,-1.13094119100209,7.52));
#8491=CARTESIAN_POINT('',(0.172988438920056,-1.65,7.52));
#8492=CARTESIAN_POINT('Origin',(0.,-1.25,7.52));
#8493=CARTESIAN_POINT('Origin',(0.,-1.25,7.52));
#8494=CARTESIAN_POINT('',(-0.172988438920056,-1.36905880899792,7.52));
#8495=CARTESIAN_POINT('Ctrl Pts',(-0.172988438920056,-1.36905880899792,
7.52));
#8496=CARTESIAN_POINT('Ctrl Pts',(-0.165594865311314,-1.37980142239529,
7.52129192197638));
#8497=CARTESIAN_POINT('Ctrl Pts',(-0.157297138725606,-1.38968770937274,
7.52265394943905));
#8498=CARTESIAN_POINT('Ctrl Pts',(-0.129892073845076,-1.41709277425327,
7.5267480843909));
#8499=CARTESIAN_POINT('Ctrl Pts',(-0.106330167759284,-1.43324205633295,
7.52969589327638));
#8500=CARTESIAN_POINT('Ctrl Pts',(-0.0546129046324105,-1.45469779396491,
7.53385029472357));
#8501=CARTESIAN_POINT('Ctrl Pts',(-0.0264512308298517,-1.46,7.535));
#8502=CARTESIAN_POINT('Ctrl Pts',(0.0264512308298516,-1.46,7.535));
#8503=CARTESIAN_POINT('Ctrl Pts',(0.0546129046324104,-1.45469779396491,
7.53385029472357));
#8504=CARTESIAN_POINT('Ctrl Pts',(0.106330167759284,-1.43324205633295,7.52969589327638));
#8505=CARTESIAN_POINT('Ctrl Pts',(0.129892073845076,-1.41709277425327,7.5267480843909));
#8506=CARTESIAN_POINT('Ctrl Pts',(0.157297138725606,-1.38968770937274,7.52265394943905));
#8507=CARTESIAN_POINT('Ctrl Pts',(0.165594865311315,-1.37980142239529,7.52129192197638));
#8508=CARTESIAN_POINT('Ctrl Pts',(0.172988438920056,-1.36905880899792,7.52));
#8509=CARTESIAN_POINT('',(-0.21,-1.25,7.52));
#8510=CARTESIAN_POINT('Origin',(0.,-1.25,7.52));
#8511=CARTESIAN_POINT('',(-0.21,-1.25,8.01522725533839));
#8512=CARTESIAN_POINT('',(-0.21,-1.25,7.52));
#8513=CARTESIAN_POINT('',(0.21,-1.25,8.01522725533839));
#8514=CARTESIAN_POINT('Ctrl Pts',(0.21,-1.25,8.01522725533839));
#8515=CARTESIAN_POINT('Ctrl Pts',(0.21,-1.27640552692445,8.01522725533839));
#8516=CARTESIAN_POINT('Ctrl Pts',(0.204715737269596,-1.30454707409071,8.01600415954412));
#8517=CARTESIAN_POINT('Ctrl Pts',(0.183273763036332,-1.35627626890513,8.01880073282317));
#8518=CARTESIAN_POINT('Ctrl Pts',(0.167117923970394,-1.37986692412796,8.02077897157582));
#8519=CARTESIAN_POINT('Ctrl Pts',(0.129867169887369,-1.41711767821098,8.02448481141327));
#8520=CARTESIAN_POINT('Ctrl Pts',(0.106276408305765,-1.43327371000135,8.02645455657129));
#8521=CARTESIAN_POINT('Ctrl Pts',(0.0545468514059001,-1.45471582482622,
8.02923165515645));
#8522=CARTESIAN_POINT('Ctrl Pts',(0.0264051785092814,-1.46,8.03));
#8523=CARTESIAN_POINT('Ctrl Pts',(-0.0264051785092814,-1.46,8.03));
#8524=CARTESIAN_POINT('Ctrl Pts',(-0.0545468514059,-1.45471582482622,8.02923165515645));
#8525=CARTESIAN_POINT('Ctrl Pts',(-0.106276408305765,-1.43327371000135,
8.02645455657129));
#8526=CARTESIAN_POINT('Ctrl Pts',(-0.129867169887369,-1.41711767821098,
8.02448481141327));
#8527=CARTESIAN_POINT('Ctrl Pts',(-0.167117923970394,-1.37986692412796,
8.02077897157582));
#8528=CARTESIAN_POINT('Ctrl Pts',(-0.183273763036331,-1.35627626890513,
8.01880073282317));
#8529=CARTESIAN_POINT('Ctrl Pts',(-0.204715737269596,-1.30454707409071,
8.01600415954412));
#8530=CARTESIAN_POINT('Ctrl Pts',(-0.21,-1.27640552692445,8.01522725533839));
#8531=CARTESIAN_POINT('Ctrl Pts',(-0.21,-1.25,8.01522725533839));
#8532=CARTESIAN_POINT('Ctrl Pts',(-0.21,-1.25,8.01522725533839));
#8533=CARTESIAN_POINT('Ctrl Pts',(-0.21,-1.22359447307555,8.01522725533839));
#8534=CARTESIAN_POINT('Ctrl Pts',(-0.204715737269596,-1.19545292590929,
8.01600415954412));
#8535=CARTESIAN_POINT('Ctrl Pts',(-0.183273763036332,-1.14372373109487,
8.01880073282317));
#8536=CARTESIAN_POINT('Ctrl Pts',(-0.167117923970394,-1.12013307587204,
8.02077897157582));
#8537=CARTESIAN_POINT('Ctrl Pts',(-0.129867169887369,-1.08288232178902,
8.02448481141327));
#8538=CARTESIAN_POINT('Ctrl Pts',(-0.106276408305765,-1.06672628999865,
8.02645455657129));
#8539=CARTESIAN_POINT('Ctrl Pts',(-0.0545468514059001,-1.04528417517378,
8.02923165515645));
#8540=CARTESIAN_POINT('Ctrl Pts',(-0.0264051785092814,-1.04,8.03));
#8541=CARTESIAN_POINT('Ctrl Pts',(0.0264051785092814,-1.04,8.03));
#8542=CARTESIAN_POINT('Ctrl Pts',(0.0545468514059002,-1.04528417517378,
8.02923165515645));
#8543=CARTESIAN_POINT('Ctrl Pts',(0.106276408305765,-1.06672628999865,8.02645455657129));
#8544=CARTESIAN_POINT('Ctrl Pts',(0.129867169887369,-1.08288232178902,8.02448481141327));
#8545=CARTESIAN_POINT('Ctrl Pts',(0.167117923970394,-1.12013307587204,8.02077897157582));
#8546=CARTESIAN_POINT('Ctrl Pts',(0.183273763036331,-1.14372373109487,8.01880073282317));
#8547=CARTESIAN_POINT('Ctrl Pts',(0.204715737269596,-1.19545292590929,8.01600415954412));
#8548=CARTESIAN_POINT('Ctrl Pts',(0.21,-1.22359447307555,8.01522725533839));
#8549=CARTESIAN_POINT('Ctrl Pts',(0.21,-1.25,8.01522725533839));
#8550=CARTESIAN_POINT('',(-0.172988438920056,-1.13094119100209,7.52));
#8551=CARTESIAN_POINT('Origin',(0.,-1.25,7.52));
#8552=CARTESIAN_POINT('Ctrl Pts',(0.172988438920056,-1.13094119100209,7.52));
#8553=CARTESIAN_POINT('Ctrl Pts',(0.165594865311315,-1.12019857760471,7.52129192197638));
#8554=CARTESIAN_POINT('Ctrl Pts',(0.157297138725606,-1.11031229062726,7.52265394943905));
#8555=CARTESIAN_POINT('Ctrl Pts',(0.129892073845076,-1.08290722574673,7.5267480843909));
#8556=CARTESIAN_POINT('Ctrl Pts',(0.106330167759284,-1.06675794366705,7.52969589327638));
#8557=CARTESIAN_POINT('Ctrl Pts',(0.0546129046324104,-1.04530220603509,
7.53385029472357));
#8558=CARTESIAN_POINT('Ctrl Pts',(0.0264512308298516,-1.04,7.535));
#8559=CARTESIAN_POINT('Ctrl Pts',(-0.0264512308298516,-1.04,7.535));
#8560=CARTESIAN_POINT('Ctrl Pts',(-0.0546129046324104,-1.04530220603509,
7.53385029472357));
#8561=CARTESIAN_POINT('Ctrl Pts',(-0.106330167759284,-1.06675794366705,
7.52969589327638));
#8562=CARTESIAN_POINT('Ctrl Pts',(-0.129892073845076,-1.08290722574673,
7.5267480843909));
#8563=CARTESIAN_POINT('Ctrl Pts',(-0.157297138725606,-1.11031229062726,
7.52265394943905));
#8564=CARTESIAN_POINT('Ctrl Pts',(-0.165594865311315,-1.12019857760471,
7.52129192197638));
#8565=CARTESIAN_POINT('Ctrl Pts',(-0.172988438920056,-1.13094119100209,
7.52));
#8566=CARTESIAN_POINT('Origin',(0.,-1.25,7.52));
#8567=CARTESIAN_POINT('',(-0.172988438920056,-1.65,7.52));
#8568=CARTESIAN_POINT('Origin',(0.,-1.65,6.53));
#8569=CARTESIAN_POINT('',(-1.005,-0.85,6.53));
#8570=CARTESIAN_POINT('Origin',(0.,-0.85,6.53));
#8571=CARTESIAN_POINT('',(-1.005,-1.65,6.53));
#8572=CARTESIAN_POINT('',(-1.005,-1.65,6.53));
#8573=CARTESIAN_POINT('Origin',(0.,-1.65,6.53));
#8574=CARTESIAN_POINT('Origin',(0.,-1.65,6.53));
#8575=CARTESIAN_POINT('',(-1.5,-0.85,6.53));
#8576=CARTESIAN_POINT('Origin',(0.,-0.85,6.53));
#8577=CARTESIAN_POINT('',(-1.5,-1.65,6.53));
#8578=CARTESIAN_POINT('',(-1.5,-1.65,6.53));
#8579=CARTESIAN_POINT('Origin',(0.,-1.65,6.53));
#8580=CARTESIAN_POINT('Origin',(0.,-0.85,6.53));
#8581=CARTESIAN_POINT('Origin',(0.,-1.65,6.53));
#8582=CARTESIAN_POINT('',(0.,0.,0.));
#8583=CARTESIAN_POINT('Origin',(0.,22.85,7.52));
#8584=CARTESIAN_POINT('',(0.172988438920056,22.7309411910021,7.52));
#8585=CARTESIAN_POINT('',(0.172988438920056,22.9690588089979,7.52));
#8586=CARTESIAN_POINT('',(0.172988438920056,22.45,7.52));
#8587=CARTESIAN_POINT('Origin',(0.,22.85,7.52));
#8588=CARTESIAN_POINT('Origin',(0.,22.85,7.52));
#8589=CARTESIAN_POINT('',(-0.172988438920056,22.7309411910021,7.52));
#8590=CARTESIAN_POINT('Ctrl Pts',(-0.172988438920056,22.7309411910021,7.52));
#8591=CARTESIAN_POINT('Ctrl Pts',(-0.165594865311315,22.7201985776047,7.52129192197638));
#8592=CARTESIAN_POINT('Ctrl Pts',(-0.157297138725606,22.7103122906273,7.52265394943905));
#8593=CARTESIAN_POINT('Ctrl Pts',(-0.129892073845076,22.6829072257467,7.5267480843909));
#8594=CARTESIAN_POINT('Ctrl Pts',(-0.106330167759284,22.6667579436671,7.52969589327638));
#8595=CARTESIAN_POINT('Ctrl Pts',(-0.0546129046324105,22.6453022060351,
7.53385029472357));
#8596=CARTESIAN_POINT('Ctrl Pts',(-0.0264512308298518,22.64,7.535));
#8597=CARTESIAN_POINT('Ctrl Pts',(0.0264512308298517,22.64,7.535));
#8598=CARTESIAN_POINT('Ctrl Pts',(0.0546129046324104,22.6453022060351,7.53385029472357));
#8599=CARTESIAN_POINT('Ctrl Pts',(0.106330167759284,22.6667579436671,7.52969589327638));
#8600=CARTESIAN_POINT('Ctrl Pts',(0.129892073845076,22.6829072257467,7.5267480843909));
#8601=CARTESIAN_POINT('Ctrl Pts',(0.157297138725606,22.7103122906273,7.52265394943905));
#8602=CARTESIAN_POINT('Ctrl Pts',(0.165594865311316,22.7201985776047,7.52129192197638));
#8603=CARTESIAN_POINT('Ctrl Pts',(0.172988438920057,22.7309411910021,7.52));
#8604=CARTESIAN_POINT('',(-0.21,22.85,7.52));
#8605=CARTESIAN_POINT('Origin',(0.,22.85,7.52));
#8606=CARTESIAN_POINT('',(-0.21,22.85,8.01522725533839));
#8607=CARTESIAN_POINT('',(-0.21,22.85,7.52));
#8608=CARTESIAN_POINT('',(0.21,22.85,8.01522725533839));
#8609=CARTESIAN_POINT('Ctrl Pts',(0.21,22.85,8.01522725533839));
#8610=CARTESIAN_POINT('Ctrl Pts',(0.21,22.8235944730755,8.01522725533839));
#8611=CARTESIAN_POINT('Ctrl Pts',(0.204715737269595,22.7954529259093,8.01600415954412));
#8612=CARTESIAN_POINT('Ctrl Pts',(0.18327376303633,22.7437237310949,8.01880073282317));
#8613=CARTESIAN_POINT('Ctrl Pts',(0.167117923970393,22.720133075872,8.02077897157582));
#8614=CARTESIAN_POINT('Ctrl Pts',(0.129867169887369,22.682882321789,8.02448481141327));
#8615=CARTESIAN_POINT('Ctrl Pts',(0.106276408305767,22.6667262899986,8.02645455657129));
#8616=CARTESIAN_POINT('Ctrl Pts',(0.0545468514059018,22.6452841751738,8.02923165515645));
#8617=CARTESIAN_POINT('Ctrl Pts',(0.0264051785092816,22.64,8.03));
#8618=CARTESIAN_POINT('Ctrl Pts',(-0.0264051785092815,22.64,8.03));
#8619=CARTESIAN_POINT('Ctrl Pts',(-0.0545468514059018,22.6452841751738,
8.02923165515645));
#8620=CARTESIAN_POINT('Ctrl Pts',(-0.106276408305767,22.6667262899986,8.02645455657129));
#8621=CARTESIAN_POINT('Ctrl Pts',(-0.129867169887368,22.682882321789,8.02448481141327));
#8622=CARTESIAN_POINT('Ctrl Pts',(-0.167117923970393,22.720133075872,8.02077897157582));
#8623=CARTESIAN_POINT('Ctrl Pts',(-0.183273763036334,22.7437237310949,8.01880073282317));
#8624=CARTESIAN_POINT('Ctrl Pts',(-0.204715737269597,22.7954529259093,8.01600415954412));
#8625=CARTESIAN_POINT('Ctrl Pts',(-0.21,22.8235944730755,8.01522725533839));
#8626=CARTESIAN_POINT('Ctrl Pts',(-0.21,22.85,8.01522725533839));
#8627=CARTESIAN_POINT('Ctrl Pts',(-0.21,22.85,8.01522725533839));
#8628=CARTESIAN_POINT('Ctrl Pts',(-0.21,22.8764055269245,8.01522725533839));
#8629=CARTESIAN_POINT('Ctrl Pts',(-0.204715737269595,22.9045470740907,8.01600415954412));
#8630=CARTESIAN_POINT('Ctrl Pts',(-0.18327376303633,22.9562762689051,8.01880073282317));
#8631=CARTESIAN_POINT('Ctrl Pts',(-0.167117923970393,22.979866924128,8.02077897157582));
#8632=CARTESIAN_POINT('Ctrl Pts',(-0.129867169887369,23.017117678211,8.02448481141327));
#8633=CARTESIAN_POINT('Ctrl Pts',(-0.106276408305767,23.0332737100014,8.02645455657129));
#8634=CARTESIAN_POINT('Ctrl Pts',(-0.0545468514059018,23.0547158248262,
8.02923165515645));
#8635=CARTESIAN_POINT('Ctrl Pts',(-0.0264051785092816,23.06,8.03));
#8636=CARTESIAN_POINT('Ctrl Pts',(0.0264051785092815,23.06,8.03));
#8637=CARTESIAN_POINT('Ctrl Pts',(0.0545468514059019,23.0547158248262,8.02923165515645));
#8638=CARTESIAN_POINT('Ctrl Pts',(0.106276408305767,23.0332737100014,8.02645455657129));
#8639=CARTESIAN_POINT('Ctrl Pts',(0.129867169887368,23.017117678211,8.02448481141327));
#8640=CARTESIAN_POINT('Ctrl Pts',(0.167117923970393,22.979866924128,8.02077897157582));
#8641=CARTESIAN_POINT('Ctrl Pts',(0.18327376303633,22.9562762689051,8.01880073282317));
#8642=CARTESIAN_POINT('Ctrl Pts',(0.204715737269595,22.9045470740907,8.01600415954412));
#8643=CARTESIAN_POINT('Ctrl Pts',(0.21,22.8764055269245,8.01522725533839));
#8644=CARTESIAN_POINT('Ctrl Pts',(0.21,22.85,8.01522725533839));
#8645=CARTESIAN_POINT('',(-0.172988438920056,22.9690588089979,7.52));
#8646=CARTESIAN_POINT('Origin',(0.,22.85,7.52));
#8647=CARTESIAN_POINT('Ctrl Pts',(0.172988438920055,22.9690588089979,7.52));
#8648=CARTESIAN_POINT('Ctrl Pts',(0.165594865311314,22.9798014223953,7.52129192197638));
#8649=CARTESIAN_POINT('Ctrl Pts',(0.157297138725605,22.9896877093727,7.52265394943905));
#8650=CARTESIAN_POINT('Ctrl Pts',(0.129892073845076,23.0170927742533,7.5267480843909));
#8651=CARTESIAN_POINT('Ctrl Pts',(0.106330167759284,23.033242056333,7.52969589327638));
#8652=CARTESIAN_POINT('Ctrl Pts',(0.0546129046324105,23.0546977939649,7.53385029472357));
#8653=CARTESIAN_POINT('Ctrl Pts',(0.0264512308298518,23.06,7.535));
#8654=CARTESIAN_POINT('Ctrl Pts',(-0.0264512308298517,23.06,7.535));
#8655=CARTESIAN_POINT('Ctrl Pts',(-0.0546129046324079,23.0546977939649,
7.53385029472357));
#8656=CARTESIAN_POINT('Ctrl Pts',(-0.106330167759282,23.033242056333,7.52969589327638));
#8657=CARTESIAN_POINT('Ctrl Pts',(-0.129892073845076,23.0170927742533,7.5267480843909));
#8658=CARTESIAN_POINT('Ctrl Pts',(-0.157297138725605,22.9896877093727,7.52265394943905));
#8659=CARTESIAN_POINT('Ctrl Pts',(-0.165594865311314,22.9798014223953,7.52129192197638));
#8660=CARTESIAN_POINT('Ctrl Pts',(-0.172988438920055,22.9690588089979,7.52));
#8661=CARTESIAN_POINT('Origin',(0.,22.85,7.52));
#8662=CARTESIAN_POINT('',(-0.172988438920056,22.45,7.52));
#8663=CARTESIAN_POINT('Origin',(0.,22.45,6.53));
#8664=CARTESIAN_POINT('',(-1.005,23.25,6.53));
#8665=CARTESIAN_POINT('Origin',(0.,23.25,6.53));
#8666=CARTESIAN_POINT('',(-1.005,22.45,6.53));
#8667=CARTESIAN_POINT('',(-1.005,22.45,6.53));
#8668=CARTESIAN_POINT('Origin',(0.,22.45,6.53));
#8669=CARTESIAN_POINT('Origin',(0.,22.45,6.53));
#8670=CARTESIAN_POINT('',(-1.5,23.25,6.53));
#8671=CARTESIAN_POINT('Origin',(0.,23.25,6.53));
#8672=CARTESIAN_POINT('',(-1.5,22.45,6.53));
#8673=CARTESIAN_POINT('',(-1.5,22.45,6.53));
#8674=CARTESIAN_POINT('Origin',(0.,22.45,6.53));
#8675=CARTESIAN_POINT('Origin',(0.,23.25,6.53));
#8676=CARTESIAN_POINT('Origin',(0.,22.45,6.53));
#8677=CARTESIAN_POINT('',(0.,0.,0.));
#8678=CARTESIAN_POINT('Origin',(-1.,0.,0.35));
#8679=CARTESIAN_POINT('',(-1.,-0.26,0.6));
#8680=CARTESIAN_POINT('',(-1.,-0.3,0.56));
#8681=CARTESIAN_POINT('',(-1.,-0.2675,0.5925));
#8682=CARTESIAN_POINT('',(-1.,0.26,0.6));
#8683=CARTESIAN_POINT('',(-1.,0.,0.6));
#8684=CARTESIAN_POINT('',(-1.,0.3,0.56));
#8685=CARTESIAN_POINT('',(-1.,0.2675,0.5925));
#8686=CARTESIAN_POINT('',(-1.,0.3,0.04));
#8687=CARTESIAN_POINT('',(-1.,0.3,0.175));
#8688=CARTESIAN_POINT('',(-1.,0.26,0.));
#8689=CARTESIAN_POINT('',(-1.,0.2925,0.0325));
#8690=CARTESIAN_POINT('',(-1.,-0.26,0.));
#8691=CARTESIAN_POINT('',(-1.,0.,0.));
#8692=CARTESIAN_POINT('',(-1.,-0.3,0.04));
#8693=CARTESIAN_POINT('',(-1.,-0.2925,0.0325));
#8694=CARTESIAN_POINT('',(-1.,-0.3,0.175));
#8695=CARTESIAN_POINT('Origin',(0.75,0.28,0.02));
#8696=CARTESIAN_POINT('',(1.,0.3,0.04));
#8697=CARTESIAN_POINT('',(0.75,0.3,0.04));
#8698=CARTESIAN_POINT('',(1.,0.26,0.));
#8699=CARTESIAN_POINT('',(1.,0.2925,0.0325));
#8700=CARTESIAN_POINT('',(0.75,0.26,0.));
#8701=CARTESIAN_POINT('Origin',(1.5,0.3,0.));
#8702=CARTESIAN_POINT('',(1.,0.3,0.56));
#8703=CARTESIAN_POINT('',(0.75,0.3,0.56));
#8704=CARTESIAN_POINT('',(1.,0.3,0.175));
#8705=CARTESIAN_POINT('Origin',(0.75,0.28,0.58));
#8706=CARTESIAN_POINT('',(1.,0.26,0.6));
#8707=CARTESIAN_POINT('',(0.75,0.26,0.6));
#8708=CARTESIAN_POINT('',(1.,0.2675,0.5925));
#8709=CARTESIAN_POINT('Origin',(0.,0.,0.6));
#8710=CARTESIAN_POINT('',(1.,-0.26,0.6));
#8711=CARTESIAN_POINT('',(-0.75,-0.26,0.6));
#8712=CARTESIAN_POINT('',(1.,0.,0.6));
#8713=CARTESIAN_POINT('Origin',(1.,0.,0.35));
#8714=CARTESIAN_POINT('',(1.,-0.26,0.));
#8715=CARTESIAN_POINT('',(1.,-0.3,0.04));
#8716=CARTESIAN_POINT('',(1.,-0.2925,0.0325));
#8717=CARTESIAN_POINT('',(1.,0.,0.));
#8718=CARTESIAN_POINT('',(1.,-0.3,0.56));
#8719=CARTESIAN_POINT('',(1.,-0.2675,0.5925));
#8720=CARTESIAN_POINT('',(1.,-0.3,0.175));
#8721=CARTESIAN_POINT('Origin',(0.,0.,0.));
#8722=CARTESIAN_POINT('',(-0.75,-0.26,0.));
#8723=CARTESIAN_POINT('Origin',(-0.75,-0.28,0.58));
#8724=CARTESIAN_POINT('',(-0.75,-0.3,0.56));
#8725=CARTESIAN_POINT('Origin',(-0.75,-0.28,0.02));
#8726=CARTESIAN_POINT('',(-0.75,-0.3,0.04));
#8727=CARTESIAN_POINT('Origin',(-1.5,-0.3,0.));
#8728=CARTESIAN_POINT('',(0.,0.,0.));
#8729=CARTESIAN_POINT('Origin',(0.375,0.5,0.));
#8730=CARTESIAN_POINT('',(-0.375,0.5,-4.59242549680257E-17));
#8731=CARTESIAN_POINT('Origin',(0.,0.5,0.));
#8732=CARTESIAN_POINT('Origin',(0.,0.475,0.));
#8733=CARTESIAN_POINT('',(-0.425,0.45,-5.20474889637625E-17));
#8734=CARTESIAN_POINT('Origin',(0.,0.45,0.));
#8735=CARTESIAN_POINT('',(-0.4,0.475,-4.89858719658941E-17));
#8736=CARTESIAN_POINT('Origin',(0.,0.24,0.));
#8737=CARTESIAN_POINT('',(-0.425,0.0299999999999998,-5.20474889637625E-17));
#8738=CARTESIAN_POINT('Origin',(0.,0.0299999999999998,0.));
#8739=CARTESIAN_POINT('',(-0.425,0.24,-5.20474889637625E-17));
#8740=CARTESIAN_POINT('Origin',(0.,0.0150000000000001,0.));
#8741=CARTESIAN_POINT('',(-0.395,4.85722573273506E-17,-4.83735485663204E-17));
#8742=CARTESIAN_POINT('Origin',(0.,0.,0.));
#8743=CARTESIAN_POINT('',(-0.41,0.0150000000000001,-5.02105187650415E-17));
#8744=CARTESIAN_POINT('Origin',(0.27,0.,0.));
#8745=CARTESIAN_POINT('',(-0.27,0.,-3.30654635769785E-17));
#8746=CARTESIAN_POINT('Origin',(0.,0.,0.));
#8747=CARTESIAN_POINT('Origin',(0.,-0.02,0.));
#8748=CARTESIAN_POINT('',(-0.24505,-0.0498999999999999,3.00099698131059E-17));
#8749=CARTESIAN_POINT('Origin',(0.,-0.0498999999999999,0.));
#8750=CARTESIAN_POINT('',(-0.26,-0.02,-3.18408167778312E-17));
#8751=CARTESIAN_POINT('Origin',(0.,-0.995,0.));
#8752=CARTESIAN_POINT('',(-0.24505,-1.95495,3.00099698131059E-17));
#8753=CARTESIAN_POINT('Origin',(0.,-1.95495,0.));
#8754=CARTESIAN_POINT('',(-0.24505,-0.995,-3.00099698131059E-17));
#8755=CARTESIAN_POINT('Origin',(0.,-1.975,0.));
#8756=CARTESIAN_POINT('',(-0.2,-2.,-2.44929359829471E-17));
#8757=CARTESIAN_POINT('Origin',(0.,-2.,0.));
#8758=CARTESIAN_POINT('',(-0.225,-1.975,-2.75545529808154E-17));
#8759=CARTESIAN_POINT('Origin',(0.,-2.,0.));
#8760=CARTESIAN_POINT('Origin',(0.115470053837925,-0.5,-0.2));
#8761=CARTESIAN_POINT('',(0.23094010767585,-0.5,0.));
#8762=CARTESIAN_POINT('',(0.115470053837925,-0.5,-0.2));
#8763=CARTESIAN_POINT('',(0.23094010767585,-0.5,0.));
#8764=CARTESIAN_POINT('',(0.115470053837925,-0.8,-0.2));
#8765=CARTESIAN_POINT('',(0.115470053837925,-0.5,-0.2));
#8766=CARTESIAN_POINT('',(0.23094010767585,-0.8,0.));
#8767=CARTESIAN_POINT('',(0.23094010767585,-0.8,0.));
#8768=CARTESIAN_POINT('',(0.23094010767585,-0.5,0.));
#8769=CARTESIAN_POINT('Origin',(-0.115470053837925,-0.5,-0.2));
#8770=CARTESIAN_POINT('',(-0.115470053837925,-0.5,-0.2));
#8771=CARTESIAN_POINT('',(0.115470053837925,-0.5,-0.2));
#8772=CARTESIAN_POINT('',(-0.115470053837925,-0.8,-0.2));
#8773=CARTESIAN_POINT('',(-0.115470053837925,-0.5,-0.2));
#8774=CARTESIAN_POINT('',(0.115470053837925,-0.8,-0.2));
#8775=CARTESIAN_POINT('Origin',(-0.23094010767585,-0.5,-2.77555756156289E-17));
#8776=CARTESIAN_POINT('',(-0.23094010767585,-0.5,-2.82820063659975E-17));
#8777=CARTESIAN_POINT('',(-0.115470053837925,-0.5,-0.2));
#8778=CARTESIAN_POINT('',(-0.23094010767585,-0.8,-2.77555756156289E-17));
#8779=CARTESIAN_POINT('',(-0.23094010767585,-0.5,-2.82820063659975E-17));
#8780=CARTESIAN_POINT('',(-0.115470053837925,-0.8,-0.2));
#8781=CARTESIAN_POINT('Origin',(-0.115470053837925,-0.5,0.2));
#8782=CARTESIAN_POINT('',(-0.115470053837925,-0.5,0.2));
#8783=CARTESIAN_POINT('',(-0.23094010767585,-0.5,-2.82820063659975E-17));
#8784=CARTESIAN_POINT('',(-0.115470053837925,-0.8,0.2));
#8785=CARTESIAN_POINT('',(-0.115470053837925,-0.5,0.2));
#8786=CARTESIAN_POINT('',(-0.23094010767585,-0.8,-2.82820063659975E-17));
#8787=CARTESIAN_POINT('Origin',(0.115470053837925,-0.5,0.2));
#8788=CARTESIAN_POINT('',(0.115470053837925,-0.5,0.2));
#8789=CARTESIAN_POINT('',(-0.115470053837925,-0.5,0.2));
#8790=CARTESIAN_POINT('',(0.115470053837925,-0.8,0.2));
#8791=CARTESIAN_POINT('',(0.115470053837925,-0.5,0.2));
#8792=CARTESIAN_POINT('',(-0.115470053837925,-0.8,0.2));
#8793=CARTESIAN_POINT('Origin',(0.23094010767585,-0.5,0.));
#8794=CARTESIAN_POINT('',(0.115470053837925,-0.5,0.2));
#8795=CARTESIAN_POINT('',(0.115470053837925,-0.8,0.2));
#8796=CARTESIAN_POINT('Origin',(0.,-0.5,0.));
#8797=CARTESIAN_POINT('Origin',(0.,-0.8,0.));
#8798=CARTESIAN_POINT('',(0.,0.,0.));
#8799=CARTESIAN_POINT('Origin',(0.45,0.6,0.));
#8800=CARTESIAN_POINT('',(-0.45,0.6,-5.51091059616309E-17));
#8801=CARTESIAN_POINT('Origin',(0.,0.6,0.));
#8802=CARTESIAN_POINT('Origin',(0.,0.575,0.));
#8803=CARTESIAN_POINT('',(-0.5,0.55,-6.12323399573677E-17));
#8804=CARTESIAN_POINT('Origin',(0.,0.55,0.));
#8805=CARTESIAN_POINT('',(-0.475,0.575,-5.81707229594993E-17));
#8806=CARTESIAN_POINT('Origin',(0.,0.29,0.));
#8807=CARTESIAN_POINT('',(-0.5,0.0299999999999998,-6.12323399573677E-17));
#8808=CARTESIAN_POINT('Origin',(0.,0.0299999999999998,0.));
#8809=CARTESIAN_POINT('',(-0.5,0.29,-6.12323399573677E-17));
#8810=CARTESIAN_POINT('Origin',(0.,0.0150000000000001,0.));
#8811=CARTESIAN_POINT('',(-0.47,7.11236625150491E-17,-5.75583995599256E-17));
#8812=CARTESIAN_POINT('Origin',(0.,0.,0.));
#8813=CARTESIAN_POINT('',(-0.485,0.0150000000000001,-5.93953697586466E-17));
#8814=CARTESIAN_POINT('Origin',(0.32,0.,0.));
#8815=CARTESIAN_POINT('',(-0.32,-6.93889390390723E-18,-3.91886975727153E-17));
#8816=CARTESIAN_POINT('Origin',(0.,0.,0.));
#8817=CARTESIAN_POINT('Origin',(0.,-0.02,0.));
#8818=CARTESIAN_POINT('',(-0.2942,-0.0515999999999999,3.60291088309151E-17));
#8819=CARTESIAN_POINT('Origin',(0.,-0.0515999999999999,0.));
#8820=CARTESIAN_POINT('',(-0.31,-0.02,-3.7964050773568E-17));
#8821=CARTESIAN_POINT('Origin',(0.,-1.24,0.));
#8822=CARTESIAN_POINT('',(-0.2942,-2.4458,3.60291088309151E-17));
#8823=CARTESIAN_POINT('Origin',(0.,-2.4458,0.));
#8824=CARTESIAN_POINT('',(-0.2942,-1.24,-3.60291088309151E-17));
#8825=CARTESIAN_POINT('Origin',(0.,-2.47,0.));
#8826=CARTESIAN_POINT('',(-0.24,-2.5,-2.93915231795365E-17));
#8827=CARTESIAN_POINT('Origin',(0.,-2.5,0.));
#8828=CARTESIAN_POINT('',(-0.27,-2.47,-3.30654635769785E-17));
#8829=CARTESIAN_POINT('Origin',(0.,-2.5,0.));
#8830=CARTESIAN_POINT('Origin',(0.144337567297406,-0.6,-0.25));
#8831=CARTESIAN_POINT('',(0.288675134594813,-0.6,0.));
#8832=CARTESIAN_POINT('',(0.144337567297406,-0.6,-0.25));
#8833=CARTESIAN_POINT('',(0.288675134594813,-0.6,0.));
#8834=CARTESIAN_POINT('',(0.144337567297406,-0.96,-0.25));
#8835=CARTESIAN_POINT('',(0.144337567297406,-0.6,-0.25));
#8836=CARTESIAN_POINT('',(0.288675134594813,-0.96,0.));
#8837=CARTESIAN_POINT('',(0.288675134594813,-0.96,0.));
#8838=CARTESIAN_POINT('',(0.288675134594813,-0.6,0.));
#8839=CARTESIAN_POINT('Origin',(-0.144337567297406,-0.6,-0.25));
#8840=CARTESIAN_POINT('',(-0.144337567297406,-0.6,-0.25));
#8841=CARTESIAN_POINT('',(0.144337567297406,-0.6,-0.25));
#8842=CARTESIAN_POINT('',(-0.144337567297406,-0.96,-0.25));
#8843=CARTESIAN_POINT('',(-0.144337567297406,-0.6,-0.25));
#8844=CARTESIAN_POINT('',(0.144337567297406,-0.96,-0.25));
#8845=CARTESIAN_POINT('Origin',(-0.288675134594813,-0.6,-8.32667268468867E-17));
#8846=CARTESIAN_POINT('',(-0.288675134594813,-0.6,-3.53525079574969E-17));
#8847=CARTESIAN_POINT('',(-0.144337567297406,-0.6,-0.25));
#8848=CARTESIAN_POINT('',(-0.288675134594813,-0.96,-5.55111512312578E-17));
#8849=CARTESIAN_POINT('',(-0.288675134594813,-0.6,-3.53525079574969E-17));
#8850=CARTESIAN_POINT('',(-0.144337567297406,-0.96,-0.25));
#8851=CARTESIAN_POINT('Origin',(-0.144337567297407,-0.6,0.25));
#8852=CARTESIAN_POINT('',(-0.144337567297407,-0.6,0.25));
#8853=CARTESIAN_POINT('',(-0.288675134594813,-0.6,-3.53525079574969E-17));
#8854=CARTESIAN_POINT('',(-0.144337567297407,-0.96,0.25));
#8855=CARTESIAN_POINT('',(-0.144337567297407,-0.6,0.25));
#8856=CARTESIAN_POINT('',(-0.288675134594813,-0.96,-3.53525079574969E-17));
#8857=CARTESIAN_POINT('Origin',(0.144337567297406,-0.6,0.25));
#8858=CARTESIAN_POINT('',(0.144337567297406,-0.6,0.25));
#8859=CARTESIAN_POINT('',(-0.144337567297407,-0.6,0.25));
#8860=CARTESIAN_POINT('',(0.144337567297406,-0.96,0.25));
#8861=CARTESIAN_POINT('',(0.144337567297406,-0.6,0.25));
#8862=CARTESIAN_POINT('',(-0.144337567297407,-0.96,0.25));
#8863=CARTESIAN_POINT('Origin',(0.288675134594813,-0.6,0.));
#8864=CARTESIAN_POINT('',(0.144337567297406,-0.6,0.25));
#8865=CARTESIAN_POINT('',(0.144337567297406,-0.96,0.25));
#8866=CARTESIAN_POINT('Origin',(0.,-0.6,0.));
#8867=CARTESIAN_POINT('Origin',(0.,-0.96,0.));
#8868=CARTESIAN_POINT('',(0.,0.,0.));
#8869=CARTESIAN_POINT('Origin',(0.,0.,0.));
#8870=CARTESIAN_POINT('',(-0.32,0.16,3.91886975727153E-17));
#8871=CARTESIAN_POINT('Origin',(0.,0.16,0.));
#8872=CARTESIAN_POINT('',(-0.32,0.,3.91886975727153E-17));
#8873=CARTESIAN_POINT('',(-0.32,0.,3.91886975727153E-17));
#8874=CARTESIAN_POINT('Origin',(0.,0.,0.));
#8875=CARTESIAN_POINT('Origin',(0.,0.,0.));
#8876=CARTESIAN_POINT('',(-0.6,0.16,7.34788079488412E-17));
#8877=CARTESIAN_POINT('Origin',(0.,0.16,0.));
#8878=CARTESIAN_POINT('',(-0.6,0.,7.34788079488412E-17));
#8879=CARTESIAN_POINT('',(-0.6,0.,7.34788079488412E-17));
#8880=CARTESIAN_POINT('Origin',(0.,0.,0.));
#8881=CARTESIAN_POINT('Origin',(0.,0.16,0.));
#8882=CARTESIAN_POINT('Origin',(0.,0.,0.));
#8883=CARTESIAN_POINT('',(0.,0.,0.));
#8884=CARTESIAN_POINT('',(0.,0.,0.));
#8885=CARTESIAN_POINT('',(0.,0.,0.));
#8886=CARTESIAN_POINT('',(0.,0.,0.));
#8887=CARTESIAN_POINT('',(0.,0.,0.));
#8888=CARTESIAN_POINT('',(0.,0.,0.));
#8889=CARTESIAN_POINT('',(0.,0.,0.));
#8890=CARTESIAN_POINT('',(0.,0.,0.));
#8891=CARTESIAN_POINT('',(0.,0.,0.));
#8892=CARTESIAN_POINT('',(-7.3,0.,3.2));
#8893=CARTESIAN_POINT('',(-7.3,0.,3.36));
#8894=CARTESIAN_POINT('',(7.3,0.,3.2));
#8895=CARTESIAN_POINT('',(7.3,0.,3.36));
#8896=CARTESIAN_POINT('',(0.,0.,6.53));
#8897=CARTESIAN_POINT('',(-4.75,0.,4.4));
#8898=CARTESIAN_POINT('',(-4.75,0.,4.56));
#8899=CARTESIAN_POINT('',(4.75,0.,4.4));
#8900=CARTESIAN_POINT('',(4.75,0.,4.56));
#8901=CARTESIAN_POINT('',(-7.3,20.,3.2));
#8902=CARTESIAN_POINT('',(-7.3,20.,3.36));
#8903=CARTESIAN_POINT('',(7.3,20.,3.2));
#8904=CARTESIAN_POINT('',(7.3,20.,3.36));
#8905=CARTESIAN_POINT('',(0.,20.,6.53));
#8906=CARTESIAN_POINT('',(-4.75,20.,4.4));
#8907=CARTESIAN_POINT('',(-4.75,20.,4.56));
#8908=CARTESIAN_POINT('',(4.75,20.,4.4));
#8909=CARTESIAN_POINT('',(4.75,20.,4.56));
#8910=CARTESIAN_POINT('',(0.,0.,0.));
#8911=CARTESIAN_POINT('Origin',(0.,0.0584134911936118,0.));
#8912=CARTESIAN_POINT('',(-0.288675134594813,0.0590919554682611,0.5));
#8913=CARTESIAN_POINT('',(0.288675134594813,0.0590919554682611,0.5));
#8914=CARTESIAN_POINT('Ctrl Pts',(-0.288675134594813,0.0590919554682611,
0.5));
#8915=CARTESIAN_POINT('Ctrl Pts',(2.1664336991023E-12,-0.0242413778636964,
0.5));
#8916=CARTESIAN_POINT('Ctrl Pts',(0.288675134594813,0.0590919554682611,
0.5));
#8917=CARTESIAN_POINT('',(-0.577350269189626,0.0590919554682611,-7.07050159149938E-17));
#8918=CARTESIAN_POINT('Ctrl Pts',(-0.577350269189626,0.0590919554682611,
-7.07050159149938E-17));
#8919=CARTESIAN_POINT('Ctrl Pts',(-0.433012701891136,-0.0242413778636963,
0.250000000001876));
#8920=CARTESIAN_POINT('Ctrl Pts',(-0.288675134594813,0.0590919554682611,
0.5));
#8921=CARTESIAN_POINT('',(-0.475,-4.16333634234434E-17,-5.81707229594993E-17));
#8922=CARTESIAN_POINT('',(-0.576175134594813,0.0584134911936118,-7.05611034329833E-17));
#8923=CARTESIAN_POINT('Origin',(0.,0.,0.));
#8924=CARTESIAN_POINT('',(-0.288675134594813,0.0590919554682611,-0.5));
#8925=CARTESIAN_POINT('Ctrl Pts',(-0.288675134594813,0.0590919554682611,
-0.5));
#8926=CARTESIAN_POINT('Ctrl Pts',(-0.433012701893303,-0.0242413778636963,
-0.249999999998124));
#8927=CARTESIAN_POINT('Ctrl Pts',(-0.577350269189626,0.0590919554682611,
-7.07050159149938E-17));
#8928=CARTESIAN_POINT('',(0.288675134594813,0.0590919554682611,-0.5));
#8929=CARTESIAN_POINT('Ctrl Pts',(0.288675134594813,0.0590919554682611,
-0.5));
#8930=CARTESIAN_POINT('Ctrl Pts',(-2.16648921025353E-12,-0.0242413778636962,
-0.5));
#8931=CARTESIAN_POINT('Ctrl Pts',(-0.288675134594813,0.0590919554682611,
-0.5));
#8932=CARTESIAN_POINT('',(0.577350269189626,0.0590919554682611,0.));
#8933=CARTESIAN_POINT('Ctrl Pts',(0.577350269189626,0.0590919554682611,
0.));
#8934=CARTESIAN_POINT('Ctrl Pts',(0.433012701891136,-0.0242413778636963,
-0.250000000001876));
#8935=CARTESIAN_POINT('Ctrl Pts',(0.288675134594813,0.0590919554682611,
-0.5));
#8936=CARTESIAN_POINT('Ctrl Pts',(0.288675134594813,0.0590919554682611,
0.5));
#8937=CARTESIAN_POINT('Ctrl Pts',(0.433012701893303,-0.0242413778636962,
0.249999999998124));
#8938=CARTESIAN_POINT('Ctrl Pts',(0.577350269189626,0.0590919554682611,
0.));
#8939=CARTESIAN_POINT('Origin',(0.,0.461586508806388,0.));
#8940=CARTESIAN_POINT('',(-0.475,0.52,-5.81707229594993E-17));
#8941=CARTESIAN_POINT('Origin',(0.,0.52,0.));
#8942=CARTESIAN_POINT('',(-0.577350269189626,0.460908044531739,-7.07050159149938E-17));
#8943=CARTESIAN_POINT('',(-0.576175134594813,0.461586508806388,-7.05611034329833E-17));
#8944=CARTESIAN_POINT('',(-0.288675134594813,0.460908044531739,0.5));
#8945=CARTESIAN_POINT('Ctrl Pts',(-0.288675134594813,0.460908044531739,
0.5));
#8946=CARTESIAN_POINT('Ctrl Pts',(-0.433012701893303,0.544241377863696,
0.249999999998124));
#8947=CARTESIAN_POINT('Ctrl Pts',(-0.577350269189626,0.460908044531739,
-7.07050159149938E-17));
#8948=CARTESIAN_POINT('',(0.288675134594813,0.460908044531739,0.5));
#8949=CARTESIAN_POINT('Ctrl Pts',(0.288675134594813,0.460908044531739,0.5));
#8950=CARTESIAN_POINT('Ctrl Pts',(-2.16676676600969E-12,0.544241377863697,
0.5));
#8951=CARTESIAN_POINT('Ctrl Pts',(-0.288675134594813,0.460908044531739,
0.5));
#8952=CARTESIAN_POINT('',(0.577350269189626,0.460908044531739,0.));
#8953=CARTESIAN_POINT('Ctrl Pts',(0.577350269189626,0.460908044531739,0.));
#8954=CARTESIAN_POINT('Ctrl Pts',(0.433012701891136,0.544241377863696,0.250000000001876));
#8955=CARTESIAN_POINT('Ctrl Pts',(0.288675134594813,0.460908044531739,0.5));
#8956=CARTESIAN_POINT('',(0.288675134594813,0.460908044531739,-0.5));
#8957=CARTESIAN_POINT('Ctrl Pts',(0.288675134594813,0.460908044531739,-0.5));
#8958=CARTESIAN_POINT('Ctrl Pts',(0.433012701893302,0.544241377863696,-0.249999999998124));
#8959=CARTESIAN_POINT('Ctrl Pts',(0.577350269189626,0.460908044531739,0.));
#8960=CARTESIAN_POINT('',(-0.288675134594813,0.460908044531739,-0.5));
#8961=CARTESIAN_POINT('Ctrl Pts',(-0.288675134594813,0.460908044531739,
-0.5));
#8962=CARTESIAN_POINT('Ctrl Pts',(2.16660023255599E-12,0.544241377863697,
-0.5));
#8963=CARTESIAN_POINT('Ctrl Pts',(0.288675134594813,0.460908044531739,-0.5));
#8964=CARTESIAN_POINT('Ctrl Pts',(-0.577350269189626,0.460908044531739,
-7.07050159149938E-17));
#8965=CARTESIAN_POINT('Ctrl Pts',(-0.433012701891136,0.544241377863696,
-0.250000000001876));
#8966=CARTESIAN_POINT('Ctrl Pts',(-0.288675134594813,0.460908044531739,
-0.5));
#8967=CARTESIAN_POINT('Origin',(0.288675134594813,0.,-0.5));
#8968=CARTESIAN_POINT('',(-0.288675134594813,0.,-0.5));
#8969=CARTESIAN_POINT('',(0.288675134594813,0.,-0.5));
#8970=CARTESIAN_POINT('Origin',(-0.288675134594813,0.,-0.5));
#8971=CARTESIAN_POINT('',(-0.577350269189626,0.,-7.07050159149938E-17));
#8972=CARTESIAN_POINT('Origin',(-0.577350269189626,0.,-7.07050159149938E-17));
#8973=CARTESIAN_POINT('',(-0.288675134594813,0.,0.5));
#8974=CARTESIAN_POINT('Origin',(0.,0.,0.));
#8975=CARTESIAN_POINT('',(-0.25175,0.52,3.08304831685346E-17));
#8976=CARTESIAN_POINT('Origin',(0.,0.52,0.));
#8977=CARTESIAN_POINT('',(-0.25175,0.,3.08304831685346E-17));
#8978=CARTESIAN_POINT('',(-0.25175,0.,3.08304831685346E-17));
#8979=CARTESIAN_POINT('Origin',(0.,0.,0.));
#8980=CARTESIAN_POINT('Origin',(-0.288675134594813,0.,0.5));
#8981=CARTESIAN_POINT('',(0.288675134594813,0.,0.5));
#8982=CARTESIAN_POINT('Origin',(0.577350269189626,0.,0.));
#8983=CARTESIAN_POINT('',(0.577350269189626,0.,0.));
#8984=CARTESIAN_POINT('Origin',(0.288675134594813,0.,0.5));
#8985=CARTESIAN_POINT('Origin',(0.,0.52,0.));
#8986=CARTESIAN_POINT('Origin',(0.,0.,0.));
#8987=CARTESIAN_POINT('',(0.,0.,0.));
#8988=CARTESIAN_POINT('Origin',(0.0721687836487032,0.,-0.125));
#8989=CARTESIAN_POINT('',(0.0721687836487032,0.,-0.125));
#8990=CARTESIAN_POINT('',(0.144337567297406,0.,0.));
#8991=CARTESIAN_POINT('',(0.117710979560879,0.,-0.0461186027918559));
#8992=CARTESIAN_POINT('',(0.0721687836487032,-0.25,-0.125));
#8993=CARTESIAN_POINT('',(0.0721687836487032,0.,-0.125));
#8994=CARTESIAN_POINT('',(0.144337567297406,-0.25,0.));
#8995=CARTESIAN_POINT('',(0.144337567297406,-0.25,0.));
#8996=CARTESIAN_POINT('',(0.144337567297406,0.,0.));
#8997=CARTESIAN_POINT('Origin',(-0.0721687836487032,0.,-0.125));
#8998=CARTESIAN_POINT('',(-0.0721687836487032,0.,-0.125));
#8999=CARTESIAN_POINT('',(0.0739156081756484,0.,-0.125));
#9000=CARTESIAN_POINT('',(-0.0721687836487032,-0.25,-0.125));
#9001=CARTESIAN_POINT('',(-0.0721687836487032,0.,-0.125));
#9002=CARTESIAN_POINT('',(0.0721687836487032,-0.25,-0.125));
#9003=CARTESIAN_POINT('Origin',(-0.144337567297406,0.,-4.16333634234434E-17));
#9004=CARTESIAN_POINT('',(-0.144337567297406,0.,-1.76762539787485E-17));
#9005=CARTESIAN_POINT('',(-0.0987953713852306,0.,-0.0788813972081442));
#9006=CARTESIAN_POINT('',(-0.144337567297406,-0.25,-2.77555756156289E-17));
#9007=CARTESIAN_POINT('',(-0.144337567297406,0.,-1.76762539787485E-17));
#9008=CARTESIAN_POINT('',(-0.0721687836487032,-0.25,-0.125));
#9009=CARTESIAN_POINT('Origin',(-0.0721687836487033,0.,0.125));
#9010=CARTESIAN_POINT('',(-0.0721687836487033,0.,0.125));
#9011=CARTESIAN_POINT('',(-0.0627109795608791,0.,0.141381397208144));
#9012=CARTESIAN_POINT('',(-0.0721687836487033,-0.25,0.125));
#9013=CARTESIAN_POINT('',(-0.0721687836487033,0.,0.125));
#9014=CARTESIAN_POINT('',(-0.144337567297406,-0.25,-1.76762539787485E-17));
#9015=CARTESIAN_POINT('Origin',(0.0721687836487032,0.,0.125));
#9016=CARTESIAN_POINT('',(0.0721687836487032,0.,0.125));
#9017=CARTESIAN_POINT('',(0.146084391824352,0.,0.125));
#9018=CARTESIAN_POINT('',(0.0721687836487032,-0.25,0.125));
#9019=CARTESIAN_POINT('',(0.0721687836487032,0.,0.125));
#9020=CARTESIAN_POINT('',(-0.0721687836487033,-0.25,0.125));
#9021=CARTESIAN_POINT('Origin',(0.144337567297406,0.,0.));
#9022=CARTESIAN_POINT('',(0.153795371385231,0.,-0.0163813972081441));
#9023=CARTESIAN_POINT('',(0.0721687836487032,-0.25,0.125));
#9024=CARTESIAN_POINT('Origin',(0.,-0.25,0.));
#9025=CARTESIAN_POINT('Origin',(0.22,0.,0.));
#9026=CARTESIAN_POINT('',(-0.22,-8.67361737988404E-18,-2.69422295812418E-17));
#9027=CARTESIAN_POINT('Origin',(0.,0.,0.));
#9028=CARTESIAN_POINT('Origin',(0.,-0.015,0.));
#9029=CARTESIAN_POINT('',(-0.24505,-0.02505,-3.00099698131059E-17));
#9030=CARTESIAN_POINT('Origin',(0.,-0.02505,0.));
#9031=CARTESIAN_POINT('',(-0.235,-0.015,-2.87791997799628E-17));
#9032=CARTESIAN_POINT('Origin',(0.,-0.3775,0.));
#9033=CARTESIAN_POINT('',(-0.24505,-0.72995,3.00099698131059E-17));
#9034=CARTESIAN_POINT('Origin',(0.,-0.72995,0.));
#9035=CARTESIAN_POINT('',(-0.24505,-0.3775,-3.00099698131059E-17));
#9036=CARTESIAN_POINT('Origin',(0.,-0.7625,0.));
#9037=CARTESIAN_POINT('',(-0.175,-0.8,-2.14313189850787E-17));
#9038=CARTESIAN_POINT('Origin',(0.,-0.8,0.));
#9039=CARTESIAN_POINT('',(-0.2125,-0.7625,-2.60237444818813E-17));
#9040=CARTESIAN_POINT('Origin',(0.,-0.8,0.));
#9041=CARTESIAN_POINT('',(0.,0.,0.));
#9042=CARTESIAN_POINT('',(0.,0.,0.));
#9043=CARTESIAN_POINT('',(0.,0.,0.));
#9044=CARTESIAN_POINT('',(0.,0.,0.));
#9045=CARTESIAN_POINT('',(0.,0.,0.));
#9046=CARTESIAN_POINT('',(0.,0.,0.));
#9047=CARTESIAN_POINT('',(0.,0.,0.));
#9048=CARTESIAN_POINT('',(0.,0.,0.));
#9049=CARTESIAN_POINT('',(0.,0.,0.));
#9050=CARTESIAN_POINT('',(0.,8.2,5.88));
#9051=CARTESIAN_POINT('',(0.,8.2,8.33));
#9052=CARTESIAN_POINT('',(0.,-4.7,6.53));
#9053=CARTESIAN_POINT('',(1.97215226305253E-31,11.8,5.88));
#9054=CARTESIAN_POINT('',(0.,11.8,8.33));
#9055=CARTESIAN_POINT('',(0.,24.7,6.53));
#9056=CARTESIAN_POINT('',(2.12132034355964,9.24,8.65132034355964));
#9057=CARTESIAN_POINT('',(2.12132034355964,9.24,8.65132034355964));
#9058=CARTESIAN_POINT('',(2.12132034355964,10.6,8.65132034355964));
#9059=CARTESIAN_POINT('',(2.12132034355964,10.76,8.65132034355964));
#9060=CARTESIAN_POINT('',(-2.12132034355964,9.24,8.65132034355964));
#9061=CARTESIAN_POINT('',(-2.12132034355964,9.24,8.65132034355964));
#9062=CARTESIAN_POINT('',(-2.12132034355964,10.6,8.65132034355964));
#9063=CARTESIAN_POINT('',(-2.12132034355964,10.76,8.65132034355964));
#9064=CARTESIAN_POINT('',(-2.12132034355964,9.24,4.40867965644036));
#9065=CARTESIAN_POINT('',(-2.12132034355964,9.24,4.40867965644036));
#9066=CARTESIAN_POINT('',(-2.12132034355964,10.6,4.40867965644036));
#9067=CARTESIAN_POINT('',(-2.12132034355964,10.76,4.40867965644036));
#9068=CARTESIAN_POINT('',(2.12132034355964,9.24,4.40867965644036));
#9069=CARTESIAN_POINT('',(2.12132034355964,9.24,4.40867965644036));
#9070=CARTESIAN_POINT('',(2.12132034355964,10.6,4.40867965644036));
#9071=CARTESIAN_POINT('',(2.12132034355964,10.76,4.40867965644036));
#9072=CARTESIAN_POINT('',(0.,-1.25,8.33));
#9073=CARTESIAN_POINT('',(0.,22.85,8.33));
#9074=CARTESIAN_POINT('',(0.,0.,0.));
#9075=CARTESIAN_POINT('',(0.,0.,0.));
#9076=UNCERTAINTY_MEASURE_WITH_UNIT(LENGTH_MEASURE(0.001),#9142,
'DISTANCE_ACCURACY_VALUE',
'Maximum model space distance between geometric entities at asserted c
onnectivities');
#9077=UNCERTAINTY_MEASURE_WITH_UNIT(LENGTH_MEASURE(0.001),#9142,
'DISTANCE_ACCURACY_VALUE',
'Maximum model space distance between geometric entities at asserted c
onnectivities');
#9078=UNCERTAINTY_MEASURE_WITH_UNIT(LENGTH_MEASURE(0.001),#9142,
'DISTANCE_ACCURACY_VALUE',
'Maximum model space distance between geometric entities at asserted c
onnectivities');
#9079=UNCERTAINTY_MEASURE_WITH_UNIT(LENGTH_MEASURE(0.001),#9142,
'DISTANCE_ACCURACY_VALUE',
'Maximum model space distance between geometric entities at asserted c
onnectivities');
#9080=UNCERTAINTY_MEASURE_WITH_UNIT(LENGTH_MEASURE(0.001),#9142,
'DISTANCE_ACCURACY_VALUE',
'Maximum model space distance between geometric entities at asserted c
onnectivities');
#9081=UNCERTAINTY_MEASURE_WITH_UNIT(LENGTH_MEASURE(0.001),#9142,
'DISTANCE_ACCURACY_VALUE',
'Maximum model space distance between geometric entities at asserted c
onnectivities');
#9082=UNCERTAINTY_MEASURE_WITH_UNIT(LENGTH_MEASURE(0.001),#9142,
'DISTANCE_ACCURACY_VALUE',
'Maximum model space distance between geometric entities at asserted c
onnectivities');
#9083=UNCERTAINTY_MEASURE_WITH_UNIT(LENGTH_MEASURE(0.001),#9142,
'DISTANCE_ACCURACY_VALUE',
'Maximum model space distance between geometric entities at asserted c
onnectivities');
#9084=UNCERTAINTY_MEASURE_WITH_UNIT(LENGTH_MEASURE(0.001),#9142,
'DISTANCE_ACCURACY_VALUE',
'Maximum model space distance between geometric entities at asserted c
onnectivities');
#9085=UNCERTAINTY_MEASURE_WITH_UNIT(LENGTH_MEASURE(0.001),#9142,
'DISTANCE_ACCURACY_VALUE',
'Maximum model space distance between geometric entities at asserted c
onnectivities');
#9086=UNCERTAINTY_MEASURE_WITH_UNIT(LENGTH_MEASURE(0.001),#9142,
'DISTANCE_ACCURACY_VALUE',
'Maximum model space distance between geometric entities at asserted c
onnectivities');
#9087=UNCERTAINTY_MEASURE_WITH_UNIT(LENGTH_MEASURE(0.001),#9142,
'DISTANCE_ACCURACY_VALUE',
'Maximum model space distance between geometric entities at asserted c
onnectivities');
#9088=UNCERTAINTY_MEASURE_WITH_UNIT(LENGTH_MEASURE(0.001),#9142,
'DISTANCE_ACCURACY_VALUE',
'Maximum model space distance between geometric entities at asserted c
onnectivities');
#9089=UNCERTAINTY_MEASURE_WITH_UNIT(LENGTH_MEASURE(0.001),#9142,
'DISTANCE_ACCURACY_VALUE',
'Maximum model space distance between geometric entities at asserted c
onnectivities');
#9090=UNCERTAINTY_MEASURE_WITH_UNIT(LENGTH_MEASURE(0.001),#9142,
'DISTANCE_ACCURACY_VALUE',
'Maximum model space distance between geometric entities at asserted c
onnectivities');
#9091=UNCERTAINTY_MEASURE_WITH_UNIT(LENGTH_MEASURE(0.001),#9142,
'DISTANCE_ACCURACY_VALUE',
'Maximum model space distance between geometric entities at asserted c
onnectivities');
#9092=UNCERTAINTY_MEASURE_WITH_UNIT(LENGTH_MEASURE(0.001),#9142,
'DISTANCE_ACCURACY_VALUE',
'Maximum model space distance between geometric entities at asserted c
onnectivities');
#9093=UNCERTAINTY_MEASURE_WITH_UNIT(LENGTH_MEASURE(0.001),#9142,
'DISTANCE_ACCURACY_VALUE',
'Maximum model space distance between geometric entities at asserted c
onnectivities');
#9094=UNCERTAINTY_MEASURE_WITH_UNIT(LENGTH_MEASURE(0.001),#9142,
'DISTANCE_ACCURACY_VALUE',
'Maximum model space distance between geometric entities at asserted c
onnectivities');
#9095=UNCERTAINTY_MEASURE_WITH_UNIT(LENGTH_MEASURE(0.001),#9142,
'DISTANCE_ACCURACY_VALUE',
'Maximum model space distance between geometric entities at asserted c
onnectivities');
#9096=UNCERTAINTY_MEASURE_WITH_UNIT(LENGTH_MEASURE(0.001),#9142,
'DISTANCE_ACCURACY_VALUE',
'Maximum model space distance between geometric entities at asserted c
onnectivities');
#9097=UNCERTAINTY_MEASURE_WITH_UNIT(LENGTH_MEASURE(0.001),#9142,
'DISTANCE_ACCURACY_VALUE',
'Maximum model space distance between geometric entities at asserted c
onnectivities');
#9098=UNCERTAINTY_MEASURE_WITH_UNIT(LENGTH_MEASURE(0.001),#9142,
'DISTANCE_ACCURACY_VALUE',
'Maximum model space distance between geometric entities at asserted c
onnectivities');
#9099=UNCERTAINTY_MEASURE_WITH_UNIT(LENGTH_MEASURE(0.001),#9142,
'DISTANCE_ACCURACY_VALUE',
'Maximum model space distance between geometric entities at asserted c
onnectivities');
#9100=UNCERTAINTY_MEASURE_WITH_UNIT(LENGTH_MEASURE(0.001),#9142,
'DISTANCE_ACCURACY_VALUE',
'Maximum model space distance between geometric entities at asserted c
onnectivities');
#9101=UNCERTAINTY_MEASURE_WITH_UNIT(LENGTH_MEASURE(0.001),#9142,
'DISTANCE_ACCURACY_VALUE',
'Maximum model space distance between geometric entities at asserted c
onnectivities');
#9102=UNCERTAINTY_MEASURE_WITH_UNIT(LENGTH_MEASURE(0.001),#9142,
'DISTANCE_ACCURACY_VALUE',
'Maximum model space distance between geometric entities at asserted c
onnectivities');
#9103=UNCERTAINTY_MEASURE_WITH_UNIT(LENGTH_MEASURE(0.001),#9142,
'DISTANCE_ACCURACY_VALUE',
'Maximum model space distance between geometric entities at asserted c
onnectivities');
#9104=UNCERTAINTY_MEASURE_WITH_UNIT(LENGTH_MEASURE(0.001),#9142,
'DISTANCE_ACCURACY_VALUE',
'Maximum model space distance between geometric entities at asserted c
onnectivities');
#9105=UNCERTAINTY_MEASURE_WITH_UNIT(LENGTH_MEASURE(0.001),#9142,
'DISTANCE_ACCURACY_VALUE',
'Maximum model space distance between geometric entities at asserted c
onnectivities');
#9106=UNCERTAINTY_MEASURE_WITH_UNIT(LENGTH_MEASURE(0.001),#9142,
'DISTANCE_ACCURACY_VALUE',
'Maximum model space distance between geometric entities at asserted c
onnectivities');
#9107=UNCERTAINTY_MEASURE_WITH_UNIT(LENGTH_MEASURE(0.001),#9142,
'DISTANCE_ACCURACY_VALUE',
'Maximum model space distance between geometric entities at asserted c
onnectivities');
#9108=UNCERTAINTY_MEASURE_WITH_UNIT(LENGTH_MEASURE(0.001),#9142,
'DISTANCE_ACCURACY_VALUE',
'Maximum model space distance between geometric entities at asserted c
onnectivities');
#9109=(
GEOMETRIC_REPRESENTATION_CONTEXT(3)
GLOBAL_UNCERTAINTY_ASSIGNED_CONTEXT((#9076))
GLOBAL_UNIT_ASSIGNED_CONTEXT((#9142,#9144,#9145))
REPRESENTATION_CONTEXT('','3D')
);
#9110=(
GEOMETRIC_REPRESENTATION_CONTEXT(3)
GLOBAL_UNCERTAINTY_ASSIGNED_CONTEXT((#9077))
GLOBAL_UNIT_ASSIGNED_CONTEXT((#9142,#9144,#9145))
REPRESENTATION_CONTEXT('','3D')
);
#9111=(
GEOMETRIC_REPRESENTATION_CONTEXT(3)
GLOBAL_UNCERTAINTY_ASSIGNED_CONTEXT((#9078))
GLOBAL_UNIT_ASSIGNED_CONTEXT((#9142,#9144,#9145))
REPRESENTATION_CONTEXT('','3D')
);
#9112=(
GEOMETRIC_REPRESENTATION_CONTEXT(3)
GLOBAL_UNCERTAINTY_ASSIGNED_CONTEXT((#9079))
GLOBAL_UNIT_ASSIGNED_CONTEXT((#9142,#9144,#9145))
REPRESENTATION_CONTEXT('','3D')
);
#9113=(
GEOMETRIC_REPRESENTATION_CONTEXT(3)
GLOBAL_UNCERTAINTY_ASSIGNED_CONTEXT((#9080))
GLOBAL_UNIT_ASSIGNED_CONTEXT((#9142,#9144,#9145))
REPRESENTATION_CONTEXT('','3D')
);
#9114=(
GEOMETRIC_REPRESENTATION_CONTEXT(3)
GLOBAL_UNCERTAINTY_ASSIGNED_CONTEXT((#9081))
GLOBAL_UNIT_ASSIGNED_CONTEXT((#9142,#9144,#9145))
REPRESENTATION_CONTEXT('','3D')
);
#9115=(
GEOMETRIC_REPRESENTATION_CONTEXT(3)
GLOBAL_UNCERTAINTY_ASSIGNED_CONTEXT((#9082))
GLOBAL_UNIT_ASSIGNED_CONTEXT((#9142,#9144,#9145))
REPRESENTATION_CONTEXT('','3D')
);
#9116=(
GEOMETRIC_REPRESENTATION_CONTEXT(3)
GLOBAL_UNCERTAINTY_ASSIGNED_CONTEXT((#9083))
GLOBAL_UNIT_ASSIGNED_CONTEXT((#9142,#9144,#9145))
REPRESENTATION_CONTEXT('','3D')
);
#9117=(
GEOMETRIC_REPRESENTATION_CONTEXT(3)
GLOBAL_UNCERTAINTY_ASSIGNED_CONTEXT((#9084))
GLOBAL_UNIT_ASSIGNED_CONTEXT((#9142,#9144,#9145))
REPRESENTATION_CONTEXT('','3D')
);
#9118=(
GEOMETRIC_REPRESENTATION_CONTEXT(3)
GLOBAL_UNCERTAINTY_ASSIGNED_CONTEXT((#9085))
GLOBAL_UNIT_ASSIGNED_CONTEXT((#9142,#9144,#9145))
REPRESENTATION_CONTEXT('','3D')
);
#9119=(
GEOMETRIC_REPRESENTATION_CONTEXT(3)
GLOBAL_UNCERTAINTY_ASSIGNED_CONTEXT((#9086))
GLOBAL_UNIT_ASSIGNED_CONTEXT((#9142,#9144,#9145))
REPRESENTATION_CONTEXT('','3D')
);
#9120=(
GEOMETRIC_REPRESENTATION_CONTEXT(3)
GLOBAL_UNCERTAINTY_ASSIGNED_CONTEXT((#9087))
GLOBAL_UNIT_ASSIGNED_CONTEXT((#9142,#9144,#9145))
REPRESENTATION_CONTEXT('','3D')
);
#9121=(
GEOMETRIC_REPRESENTATION_CONTEXT(3)
GLOBAL_UNCERTAINTY_ASSIGNED_CONTEXT((#9088))
GLOBAL_UNIT_ASSIGNED_CONTEXT((#9142,#9144,#9145))
REPRESENTATION_CONTEXT('','3D')
);
#9122=(
GEOMETRIC_REPRESENTATION_CONTEXT(3)
GLOBAL_UNCERTAINTY_ASSIGNED_CONTEXT((#9089))
GLOBAL_UNIT_ASSIGNED_CONTEXT((#9142,#9144,#9145))
REPRESENTATION_CONTEXT('','3D')
);
#9123=(
GEOMETRIC_REPRESENTATION_CONTEXT(3)
GLOBAL_UNCERTAINTY_ASSIGNED_CONTEXT((#9090))
GLOBAL_UNIT_ASSIGNED_CONTEXT((#9142,#9144,#9145))
REPRESENTATION_CONTEXT('','3D')
);
#9124=(
GEOMETRIC_REPRESENTATION_CONTEXT(3)
GLOBAL_UNCERTAINTY_ASSIGNED_CONTEXT((#9091))
GLOBAL_UNIT_ASSIGNED_CONTEXT((#9142,#9144,#9145))
REPRESENTATION_CONTEXT('','3D')
);
#9125=(
GEOMETRIC_REPRESENTATION_CONTEXT(3)
GLOBAL_UNCERTAINTY_ASSIGNED_CONTEXT((#9092))
GLOBAL_UNIT_ASSIGNED_CONTEXT((#9142,#9144,#9145))
REPRESENTATION_CONTEXT('','3D')
);
#9126=(
GEOMETRIC_REPRESENTATION_CONTEXT(3)
GLOBAL_UNCERTAINTY_ASSIGNED_CONTEXT((#9093))
GLOBAL_UNIT_ASSIGNED_CONTEXT((#9142,#9144,#9145))
REPRESENTATION_CONTEXT('','3D')
);
#9127=(
GEOMETRIC_REPRESENTATION_CONTEXT(3)
GLOBAL_UNCERTAINTY_ASSIGNED_CONTEXT((#9094))
GLOBAL_UNIT_ASSIGNED_CONTEXT((#9142,#9144,#9145))
REPRESENTATION_CONTEXT('','3D')
);
#9128=(
GEOMETRIC_REPRESENTATION_CONTEXT(3)
GLOBAL_UNCERTAINTY_ASSIGNED_CONTEXT((#9095))
GLOBAL_UNIT_ASSIGNED_CONTEXT((#9142,#9144,#9145))
REPRESENTATION_CONTEXT('','3D')
);
#9129=(
GEOMETRIC_REPRESENTATION_CONTEXT(3)
GLOBAL_UNCERTAINTY_ASSIGNED_CONTEXT((#9096))
GLOBAL_UNIT_ASSIGNED_CONTEXT((#9142,#9144,#9145))
REPRESENTATION_CONTEXT('','3D')
);
#9130=(
GEOMETRIC_REPRESENTATION_CONTEXT(3)
GLOBAL_UNCERTAINTY_ASSIGNED_CONTEXT((#9097))
GLOBAL_UNIT_ASSIGNED_CONTEXT((#9142,#9144,#9145))
REPRESENTATION_CONTEXT('','3D')
);
#9131=(
GEOMETRIC_REPRESENTATION_CONTEXT(3)
GLOBAL_UNCERTAINTY_ASSIGNED_CONTEXT((#9098))
GLOBAL_UNIT_ASSIGNED_CONTEXT((#9142,#9144,#9145))
REPRESENTATION_CONTEXT('','3D')
);
#9132=(
GEOMETRIC_REPRESENTATION_CONTEXT(3)
GLOBAL_UNCERTAINTY_ASSIGNED_CONTEXT((#9099))
GLOBAL_UNIT_ASSIGNED_CONTEXT((#9142,#9144,#9145))
REPRESENTATION_CONTEXT('','3D')
);
#9133=(
GEOMETRIC_REPRESENTATION_CONTEXT(3)
GLOBAL_UNCERTAINTY_ASSIGNED_CONTEXT((#9100))
GLOBAL_UNIT_ASSIGNED_CONTEXT((#9142,#9144,#9145))
REPRESENTATION_CONTEXT('','3D')
);
#9134=(
GEOMETRIC_REPRESENTATION_CONTEXT(3)
GLOBAL_UNCERTAINTY_ASSIGNED_CONTEXT((#9101))
GLOBAL_UNIT_ASSIGNED_CONTEXT((#9142,#9144,#9145))
REPRESENTATION_CONTEXT('','3D')
);
#9135=(
GEOMETRIC_REPRESENTATION_CONTEXT(3)
GLOBAL_UNCERTAINTY_ASSIGNED_CONTEXT((#9102))
GLOBAL_UNIT_ASSIGNED_CONTEXT((#9142,#9144,#9145))
REPRESENTATION_CONTEXT('','3D')
);
#9136=(
GEOMETRIC_REPRESENTATION_CONTEXT(3)
GLOBAL_UNCERTAINTY_ASSIGNED_CONTEXT((#9103))
GLOBAL_UNIT_ASSIGNED_CONTEXT((#9142,#9144,#9145))
REPRESENTATION_CONTEXT('','3D')
);
#9137=(
GEOMETRIC_REPRESENTATION_CONTEXT(3)
GLOBAL_UNCERTAINTY_ASSIGNED_CONTEXT((#9104))
GLOBAL_UNIT_ASSIGNED_CONTEXT((#9142,#9144,#9145))
REPRESENTATION_CONTEXT('','3D')
);
#9138=(
GEOMETRIC_REPRESENTATION_CONTEXT(3)
GLOBAL_UNCERTAINTY_ASSIGNED_CONTEXT((#9105))
GLOBAL_UNIT_ASSIGNED_CONTEXT((#9142,#9144,#9145))
REPRESENTATION_CONTEXT('','3D')
);
#9139=(
GEOMETRIC_REPRESENTATION_CONTEXT(3)
GLOBAL_UNCERTAINTY_ASSIGNED_CONTEXT((#9106))
GLOBAL_UNIT_ASSIGNED_CONTEXT((#9142,#9144,#9145))
REPRESENTATION_CONTEXT('','3D')
);
#9140=(
GEOMETRIC_REPRESENTATION_CONTEXT(3)
GLOBAL_UNCERTAINTY_ASSIGNED_CONTEXT((#9107))
GLOBAL_UNIT_ASSIGNED_CONTEXT((#9142,#9144,#9145))
REPRESENTATION_CONTEXT('','3D')
);
#9141=(
GEOMETRIC_REPRESENTATION_CONTEXT(3)
GLOBAL_UNCERTAINTY_ASSIGNED_CONTEXT((#9108))
GLOBAL_UNIT_ASSIGNED_CONTEXT((#9142,#9144,#9145))
REPRESENTATION_CONTEXT('','3D')
);
#9142=(
LENGTH_UNIT()
NAMED_UNIT(*)
SI_UNIT(.CENTI.,.METRE.)
);
#9143=(
LENGTH_UNIT()
NAMED_UNIT(*)
SI_UNIT($,.METRE.)
);
#9144=(
NAMED_UNIT(*)
PLANE_ANGLE_UNIT()
SI_UNIT($,.RADIAN.)
);
#9145=(
NAMED_UNIT(*)
SI_UNIT($,.STERADIAN.)
SOLID_ANGLE_UNIT()
);
#9146=SHAPE_DEFINITION_REPRESENTATION(#9178,#9274);
#9147=SHAPE_DEFINITION_REPRESENTATION(#9179,#9275);
#9148=SHAPE_DEFINITION_REPRESENTATION(#9180,#9276);
#9149=SHAPE_DEFINITION_REPRESENTATION(#9181,#9277);
#9150=SHAPE_DEFINITION_REPRESENTATION(#9182,#9278);
#9151=SHAPE_DEFINITION_REPRESENTATION(#9183,#9279);
#9152=SHAPE_DEFINITION_REPRESENTATION(#9184,#9280);
#9153=SHAPE_DEFINITION_REPRESENTATION(#9185,#9281);
#9154=SHAPE_DEFINITION_REPRESENTATION(#9186,#9282);
#9155=SHAPE_DEFINITION_REPRESENTATION(#9187,#9283);
#9156=SHAPE_DEFINITION_REPRESENTATION(#9188,#9284);
#9157=SHAPE_DEFINITION_REPRESENTATION(#9189,#9285);
#9158=SHAPE_DEFINITION_REPRESENTATION(#9190,#9286);
#9159=SHAPE_DEFINITION_REPRESENTATION(#9191,#9287);
#9160=SHAPE_DEFINITION_REPRESENTATION(#9194,#9288);
#9161=SHAPE_DEFINITION_REPRESENTATION(#9195,#9289);
#9162=SHAPE_DEFINITION_REPRESENTATION(#9196,#9290);
#9163=SHAPE_DEFINITION_REPRESENTATION(#9197,#9291);
#9164=SHAPE_DEFINITION_REPRESENTATION(#9198,#9292);
#9165=SHAPE_DEFINITION_REPRESENTATION(#9199,#9293);
#9166=SHAPE_DEFINITION_REPRESENTATION(#9200,#9294);
#9167=SHAPE_DEFINITION_REPRESENTATION(#9201,#9295);
#9168=SHAPE_DEFINITION_REPRESENTATION(#9202,#9296);
#9169=SHAPE_DEFINITION_REPRESENTATION(#9203,#9297);
#9170=SHAPE_DEFINITION_REPRESENTATION(#9204,#9298);
#9171=SHAPE_DEFINITION_REPRESENTATION(#9205,#9299);
#9172=SHAPE_DEFINITION_REPRESENTATION(#9206,#9300);
#9173=SHAPE_DEFINITION_REPRESENTATION(#9207,#9301);
#9174=SHAPE_DEFINITION_REPRESENTATION(#9208,#9302);
#9175=SHAPE_DEFINITION_REPRESENTATION(#9209,#9303);
#9176=SHAPE_DEFINITION_REPRESENTATION(#9237,#9304);
#9177=SHAPE_DEFINITION_REPRESENTATION(#9238,#9305);
#9178=PRODUCT_DEFINITION_SHAPE('',$,#9307);
#9179=PRODUCT_DEFINITION_SHAPE('',$,#9308);
#9180=PRODUCT_DEFINITION_SHAPE('',$,#9309);
#9181=PRODUCT_DEFINITION_SHAPE('',$,#9310);
#9182=PRODUCT_DEFINITION_SHAPE('',$,#9311);
#9183=PRODUCT_DEFINITION_SHAPE('',$,#9312);
#9184=PRODUCT_DEFINITION_SHAPE('',$,#9313);
#9185=PRODUCT_DEFINITION_SHAPE('',$,#9314);
#9186=PRODUCT_DEFINITION_SHAPE('',$,#9315);
#9187=PRODUCT_DEFINITION_SHAPE('',$,#9316);
#9188=PRODUCT_DEFINITION_SHAPE('',$,#9317);
#9189=PRODUCT_DEFINITION_SHAPE('',$,#9318);
#9190=PRODUCT_DEFINITION_SHAPE('',$,#9319);
#9191=PRODUCT_DEFINITION_SHAPE('',$,#9320);
#9192=PRODUCT_DEFINITION_SHAPE($,$,#236);
#9193=PRODUCT_DEFINITION_SHAPE($,$,#237);
#9194=PRODUCT_DEFINITION_SHAPE('',$,#9321);
#9195=PRODUCT_DEFINITION_SHAPE('',$,#9322);
#9196=PRODUCT_DEFINITION_SHAPE('',$,#9323);
#9197=PRODUCT_DEFINITION_SHAPE('',$,#9324);
#9198=PRODUCT_DEFINITION_SHAPE('',$,#9325);
#9199=PRODUCT_DEFINITION_SHAPE('',$,#9326);
#9200=PRODUCT_DEFINITION_SHAPE('',$,#9327);
#9201=PRODUCT_DEFINITION_SHAPE('',$,#9328);
#9202=PRODUCT_DEFINITION_SHAPE('',$,#9329);
#9203=PRODUCT_DEFINITION_SHAPE('',$,#9330);
#9204=PRODUCT_DEFINITION_SHAPE('',$,#9331);
#9205=PRODUCT_DEFINITION_SHAPE('',$,#9332);
#9206=PRODUCT_DEFINITION_SHAPE('',$,#9333);
#9207=PRODUCT_DEFINITION_SHAPE('',$,#9334);
#9208=PRODUCT_DEFINITION_SHAPE('',$,#9335);
#9209=PRODUCT_DEFINITION_SHAPE('',$,#9336);
#9210=PRODUCT_DEFINITION_SHAPE($,$,#238);
#9211=PRODUCT_DEFINITION_SHAPE($,$,#239);
#9212=PRODUCT_DEFINITION_SHAPE($,$,#240);
#9213=PRODUCT_DEFINITION_SHAPE($,$,#241);
#9214=PRODUCT_DEFINITION_SHAPE($,$,#242);
#9215=PRODUCT_DEFINITION_SHAPE($,$,#243);
#9216=PRODUCT_DEFINITION_SHAPE($,$,#244);
#9217=PRODUCT_DEFINITION_SHAPE($,$,#245);
#9218=PRODUCT_DEFINITION_SHAPE($,$,#246);
#9219=PRODUCT_DEFINITION_SHAPE($,$,#247);
#9220=PRODUCT_DEFINITION_SHAPE($,$,#248);
#9221=PRODUCT_DEFINITION_SHAPE($,$,#249);
#9222=PRODUCT_DEFINITION_SHAPE($,$,#250);
#9223=PRODUCT_DEFINITION_SHAPE($,$,#251);
#9224=PRODUCT_DEFINITION_SHAPE($,$,#252);
#9225=PRODUCT_DEFINITION_SHAPE($,$,#253);
#9226=PRODUCT_DEFINITION_SHAPE($,$,#254);
#9227=PRODUCT_DEFINITION_SHAPE($,$,#255);
#9228=PRODUCT_DEFINITION_SHAPE($,$,#256);
#9229=PRODUCT_DEFINITION_SHAPE($,$,#257);
#9230=PRODUCT_DEFINITION_SHAPE($,$,#258);
#9231=PRODUCT_DEFINITION_SHAPE($,$,#259);
#9232=PRODUCT_DEFINITION_SHAPE($,$,#260);
#9233=PRODUCT_DEFINITION_SHAPE($,$,#261);
#9234=PRODUCT_DEFINITION_SHAPE($,$,#262);
#9235=PRODUCT_DEFINITION_SHAPE($,$,#263);
#9236=PRODUCT_DEFINITION_SHAPE($,$,#264);
#9237=PRODUCT_DEFINITION_SHAPE('',$,#9337);
#9238=PRODUCT_DEFINITION_SHAPE('',$,#9338);
#9239=PRODUCT_DEFINITION_SHAPE($,$,#265);
#9240=PRODUCT_DEFINITION_SHAPE($,$,#266);
#9241=PRODUCT_DEFINITION_SHAPE($,$,#267);
#9242=PRODUCT_DEFINITION_SHAPE($,$,#268);
#9243=PRODUCT_DEFINITION_SHAPE($,$,#269);
#9244=PRODUCT_DEFINITION_SHAPE($,$,#270);
#9245=PRODUCT_DEFINITION_SHAPE($,$,#271);
#9246=PRODUCT_DEFINITION_SHAPE($,$,#272);
#9247=PRODUCT_DEFINITION_SHAPE($,$,#273);
#9248=PRODUCT_DEFINITION_SHAPE($,$,#274);
#9249=PRODUCT_DEFINITION_SHAPE($,$,#275);
#9250=PRODUCT_DEFINITION_SHAPE($,$,#276);
#9251=PRODUCT_DEFINITION_SHAPE($,$,#277);
#9252=PRODUCT_DEFINITION_SHAPE($,$,#278);
#9253=PRODUCT_DEFINITION_SHAPE($,$,#279);
#9254=PRODUCT_DEFINITION_SHAPE($,$,#280);
#9255=PRODUCT_DEFINITION_SHAPE($,$,#281);
#9256=PRODUCT_DEFINITION_SHAPE($,$,#282);
#9257=PRODUCT_DEFINITION_SHAPE($,$,#283);
#9258=PRODUCT_DEFINITION_SHAPE($,$,#284);
#9259=PRODUCT_DEFINITION_SHAPE($,$,#285);
#9260=PRODUCT_DEFINITION_SHAPE($,$,#286);
#9261=PRODUCT_DEFINITION_SHAPE($,$,#287);
#9262=PRODUCT_DEFINITION_SHAPE($,$,#288);
#9263=PRODUCT_DEFINITION_SHAPE($,$,#289);
#9264=PRODUCT_DEFINITION_SHAPE($,$,#290);
#9265=PRODUCT_DEFINITION_SHAPE($,$,#291);
#9266=PRODUCT_DEFINITION_SHAPE($,$,#292);
#9267=PRODUCT_DEFINITION_SHAPE($,$,#293);
#9268=PRODUCT_DEFINITION_SHAPE($,$,#294);
#9269=PRODUCT_DEFINITION_SHAPE($,$,#295);
#9270=PRODUCT_DEFINITION_SHAPE($,$,#296);
#9271=PRODUCT_DEFINITION_SHAPE($,$,#297);
#9272=PRODUCT_DEFINITION_SHAPE($,$,#298);
#9273=PRODUCT_DEFINITION_SHAPE($,$,#299);
#9274=SHAPE_REPRESENTATION('',(#5093,#5640,#5641),#9109);
#9275=SHAPE_REPRESENTATION('',(#5094,#5547,#5548,#5549,#5550,#5551,#5552,
#5553,#5554,#5555,#5556,#5557,#5558,#5559,#5560,#5561,#5562,#5563,#5564,
#5565,#5566,#5567,#5568,#5569,#5570,#5571,#5572,#5573),#9110);
#9276=SHAPE_REPRESENTATION('',(#5095),#9111);
#9277=SHAPE_REPRESENTATION('',(#5114),#9112);
#9278=SHAPE_REPRESENTATION('',(#5121),#9113);
#9279=SHAPE_REPRESENTATION('',(#5128),#9114);
#9280=SHAPE_REPRESENTATION('',(#5147),#9115);
#9281=SHAPE_REPRESENTATION('',(#5156),#9116);
#9282=SHAPE_REPRESENTATION('',(#5165),#9117);
#9283=SHAPE_REPRESENTATION('',(#5184),#9118);
#9284=SHAPE_REPRESENTATION('',(#5193),#9119);
#9285=SHAPE_REPRESENTATION('',(#5202,#5272,#5273),#9120);
#9286=SHAPE_REPRESENTATION('',(#5203),#9121);
#9287=SHAPE_REPRESENTATION('',(#5244),#9122);
#9288=SHAPE_REPRESENTATION('',(#5274),#9123);
#9289=SHAPE_REPRESENTATION('',(#5283),#9124);
#9290=SHAPE_REPRESENTATION('',(#5307,#5607,#5608,#5609,#5610,#5611,#5612,
#5613,#5614,#5615,#5616,#5617,#5618,#5619,#5620,#5621,#5622,#5623,#5624,
#5625,#5626,#5627,#5628,#5629,#5630,#5631,#5632,#5633,#5634,#5635,#5636,
#5637,#5638,#5639),#9125);
#9291=SHAPE_REPRESENTATION('',(#5308),#9126);
#9292=SHAPE_REPRESENTATION('',(#5325),#9127);
#9293=SHAPE_REPRESENTATION('',(#5363),#9128);
#9294=SHAPE_REPRESENTATION('',(#5372),#9129);
#9295=SHAPE_REPRESENTATION('',(#5389),#9130);
#9296=SHAPE_REPRESENTATION('',(#5427),#9131);
#9297=SHAPE_REPRESENTATION('',(#5436),#9132);
#9298=SHAPE_REPRESENTATION('',(#5445),#9133);
#9299=SHAPE_REPRESENTATION('',(#5460),#9134);
#9300=SHAPE_REPRESENTATION('',(#5475),#9135);
#9301=SHAPE_REPRESENTATION('',(#5486),#9136);
#9302=SHAPE_REPRESENTATION('',(#5512),#9137);
#9303=SHAPE_REPRESENTATION('',(#5538),#9138);
#9304=SHAPE_REPRESENTATION('',(#5574),#9139);
#9305=SHAPE_REPRESENTATION('',(#5590),#9140);
#9306=PRODUCT_DEFINITION_CONTEXT('part definition',#9404,'design');
#9307=PRODUCT_DEFINITION('PAT-087',
'PAT-087',#9339,#9306);
#9308=PRODUCT_DEFINITION('Support frame','Support frame',#9340,#9306);
#9309=PRODUCT_DEFINITION('Base','Base',#9341,#9306);
#9310=PRODUCT_DEFINITION('Bonded pad','Bonded pad',#9342,#9306);
#9311=PRODUCT_DEFINITION('Bonded pad (1)','Bonded pad (1)',#9343,#9306);
#9312=PRODUCT_DEFINITION('Bearing riser','Bearing riser',#9344,#9306);
#9313=PRODUCT_DEFINITION('Mounting bush','Mounting bush',#9345,#9306);
#9314=PRODUCT_DEFINITION('Mounting bush (1)','Mounting bush (1)',#9346,#9306);
#9315=PRODUCT_DEFINITION('Bearing riser (1)','Bearing riser (1)',#9347,#9306);
#9316=PRODUCT_DEFINITION('Mounting bush (2)','Mounting bush (2)',#9348,#9306);
#9317=PRODUCT_DEFINITION('Mounting bush (3)','Mounting bush (3)',#9349,#9306);
#9318=PRODUCT_DEFINITION('Pillow Block Bearing - 20 mm Bore',
'Pillow Block Bearing - 20 mm Bore',#9350,#9306);
#9319=PRODUCT_DEFINITION('Housing','Housing',#9351,#9306);
#9320=PRODUCT_DEFINITION('Insert bearing','Insert bearing',#9352,#9306);
#9321=PRODUCT_DEFINITION('Flat Washer - M8','Flat Washer - M8',#9353,#9306);
#9322=PRODUCT_DEFINITION('M8x25 Bolt','M8x25 Bolt',#9354,#9306);
#9323=PRODUCT_DEFINITION('Coupled shafts','Coupled shafts',#9355,#9306);
#9324=PRODUCT_DEFINITION('Shaft stub','Shaft stub',#9356,#9306);
#9325=PRODUCT_DEFINITION('Flange A','Flange A',#9357,#9306);
#9326=PRODUCT_DEFINITION('End keeper','End keeper',#9358,#9306);
#9327=PRODUCT_DEFINITION('Shaft stub (1)','Shaft stub (1)',#9359,#9306);
#9328=PRODUCT_DEFINITION('Flange B','Flange B',#9360,#9306);
#9329=PRODUCT_DEFINITION('End keeper (1)','End keeper (1)',#9361,#9306);
#9330=PRODUCT_DEFINITION('Pilot ring','Pilot ring',#9362,#9306);
#9331=PRODUCT_DEFINITION('End collar','End collar',#9363,#9306);
#9332=PRODUCT_DEFINITION('End collar (1)','End collar (1)',#9364,#9306);
#9333=PRODUCT_DEFINITION('Key 6x6x20','Key 6x6x20',#9365,#9306);
#9334=PRODUCT_DEFINITION('Cap Screw - M5x20','Cap Screw - M5x20',#9366,
#9306);
#9335=PRODUCT_DEFINITION('Cap Screw - M6x25','Cap Screw - M6x25',#9367,
#9306);
#9336=PRODUCT_DEFINITION('Flat Washer - M6','Flat Washer - M6',#9368,#9306);
#9337=PRODUCT_DEFINITION('Hex Nut - M6','Hex Nut - M6',#9369,#9306);
#9338=PRODUCT_DEFINITION('Socket Set Screw - M5x8',
'Socket Set Screw - M5x8',#9370,#9306);
#9339=PRODUCT_DEFINITION_FORMATION('',$,#9406);
#9340=PRODUCT_DEFINITION_FORMATION('',$,#9407);
#9341=PRODUCT_DEFINITION_FORMATION('',$,#9408);
#9342=PRODUCT_DEFINITION_FORMATION('',$,#9409);
#9343=PRODUCT_DEFINITION_FORMATION('',$,#9410);
#9344=PRODUCT_DEFINITION_FORMATION('',$,#9411);
#9345=PRODUCT_DEFINITION_FORMATION('',$,#9412);
#9346=PRODUCT_DEFINITION_FORMATION('',$,#9413);
#9347=PRODUCT_DEFINITION_FORMATION('',$,#9414);
#9348=PRODUCT_DEFINITION_FORMATION('',$,#9415);
#9349=PRODUCT_DEFINITION_FORMATION('',$,#9416);
#9350=PRODUCT_DEFINITION_FORMATION('',$,#9417);
#9351=PRODUCT_DEFINITION_FORMATION('',$,#9418);
#9352=PRODUCT_DEFINITION_FORMATION('',$,#9419);
#9353=PRODUCT_DEFINITION_FORMATION('',$,#9420);
#9354=PRODUCT_DEFINITION_FORMATION('',$,#9421);
#9355=PRODUCT_DEFINITION_FORMATION('',$,#9422);
#9356=PRODUCT_DEFINITION_FORMATION('',$,#9423);
#9357=PRODUCT_DEFINITION_FORMATION('',$,#9424);
#9358=PRODUCT_DEFINITION_FORMATION('',$,#9425);
#9359=PRODUCT_DEFINITION_FORMATION('',$,#9426);
#9360=PRODUCT_DEFINITION_FORMATION('',$,#9427);
#9361=PRODUCT_DEFINITION_FORMATION('',$,#9428);
#9362=PRODUCT_DEFINITION_FORMATION('',$,#9429);
#9363=PRODUCT_DEFINITION_FORMATION('',$,#9430);
#9364=PRODUCT_DEFINITION_FORMATION('',$,#9431);
#9365=PRODUCT_DEFINITION_FORMATION('',$,#9432);
#9366=PRODUCT_DEFINITION_FORMATION('',$,#9433);
#9367=PRODUCT_DEFINITION_FORMATION('',$,#9434);
#9368=PRODUCT_DEFINITION_FORMATION('',$,#9435);
#9369=PRODUCT_DEFINITION_FORMATION('',$,#9436);
#9370=PRODUCT_DEFINITION_FORMATION('',$,#9437);
#9371=PRODUCT_RELATED_PRODUCT_CATEGORY('PAT-087','PAT-087',(#9406));
#9372=PRODUCT_RELATED_PRODUCT_CATEGORY('Support frame','Support frame',
(#9407));
#9373=PRODUCT_RELATED_PRODUCT_CATEGORY('Base','Base',(#9408));
#9374=PRODUCT_RELATED_PRODUCT_CATEGORY('Bonded pad','Bonded pad',(#9409));
#9375=PRODUCT_RELATED_PRODUCT_CATEGORY('Bonded pad (1)',
'Bonded pad (1)',(#9410));
#9376=PRODUCT_RELATED_PRODUCT_CATEGORY('Bearing riser','Bearing riser',
(#9411));
#9377=PRODUCT_RELATED_PRODUCT_CATEGORY('Mounting bush','Mounting bush',
(#9412));
#9378=PRODUCT_RELATED_PRODUCT_CATEGORY('Mounting bush (1)',
'Mounting bush (1)',(#9413));
#9379=PRODUCT_RELATED_PRODUCT_CATEGORY('Bearing riser (1)',
'Bearing riser (1)',(#9414));
#9380=PRODUCT_RELATED_PRODUCT_CATEGORY('Mounting bush (2)',
'Mounting bush (2)',(#9415));
#9381=PRODUCT_RELATED_PRODUCT_CATEGORY('Mounting bush (3)',
'Mounting bush (3)',(#9416));
#9382=PRODUCT_RELATED_PRODUCT_CATEGORY(
'Pillow Block Bearing - 20 mm Bore','Pillow Block Bearing - 20 mm Bore',
(#9417));
#9383=PRODUCT_RELATED_PRODUCT_CATEGORY('Housing','Housing',(#9418));
#9384=PRODUCT_RELATED_PRODUCT_CATEGORY('Insert bearing',
'Insert bearing',(#9419));
#9385=PRODUCT_RELATED_PRODUCT_CATEGORY('Flat Washer - M8',
'Flat Washer - M8',(#9420));
#9386=PRODUCT_RELATED_PRODUCT_CATEGORY('M8x25 Bolt','M8x25 Bolt',(#9421));
#9387=PRODUCT_RELATED_PRODUCT_CATEGORY('Coupled shafts',
'Coupled shafts',(#9422));
#9388=PRODUCT_RELATED_PRODUCT_CATEGORY('Shaft stub','Shaft stub',(#9423));
#9389=PRODUCT_RELATED_PRODUCT_CATEGORY('Flange A','Flange A',(#9424));
#9390=PRODUCT_RELATED_PRODUCT_CATEGORY('End keeper','End keeper',(#9425));
#9391=PRODUCT_RELATED_PRODUCT_CATEGORY('Shaft stub (1)',
'Shaft stub (1)',(#9426));
#9392=PRODUCT_RELATED_PRODUCT_CATEGORY('Flange B','Flange B',(#9427));
#9393=PRODUCT_RELATED_PRODUCT_CATEGORY('End keeper (1)',
'End keeper (1)',(#9428));
#9394=PRODUCT_RELATED_PRODUCT_CATEGORY('Pilot ring','Pilot ring',(#9429));
#9395=PRODUCT_RELATED_PRODUCT_CATEGORY('End collar','End collar',(#9430));
#9396=PRODUCT_RELATED_PRODUCT_CATEGORY('End collar (1)',
'End collar (1)',(#9431));
#9397=PRODUCT_RELATED_PRODUCT_CATEGORY('Key 6x6x20','Key 6x6x20',(#9432));
#9398=PRODUCT_RELATED_PRODUCT_CATEGORY('Cap Screw - M5x20',
'Cap Screw - M5x20',(#9433));
#9399=PRODUCT_RELATED_PRODUCT_CATEGORY('Cap Screw - M6x25',
'Cap Screw - M6x25',(#9434));
#9400=PRODUCT_RELATED_PRODUCT_CATEGORY('Flat Washer - M6',
'Flat Washer - M6',(#9435));
#9401=PRODUCT_RELATED_PRODUCT_CATEGORY('Hex Nut - M6','Hex Nut - M6',(#9436));
#9402=PRODUCT_RELATED_PRODUCT_CATEGORY('Socket Set Screw - M5x8',
'Socket Set Screw - M5x8',(#9437));
#9403=APPLICATION_PROTOCOL_DEFINITION('international standard',
'automotive_design',2009,#9404);
#9404=APPLICATION_CONTEXT(
'Core Data for Automotive Mechanical Design Process');
#9405=PRODUCT_CONTEXT('part definition',#9404,'mechanical');
#9406=PRODUCT('PAT-087','PAT-087',
'PAT-087',(#9405));
#9407=PRODUCT('Support frame','Support frame','Support frame',(#9405));
#9408=PRODUCT('Base','Base','Base',(#9405));
#9409=PRODUCT('Bonded pad','Bonded pad','Bonded pad',(#9405));
#9410=PRODUCT('Bonded pad (1)','Bonded pad (1)','Bonded pad (1)',(#9405));
#9411=PRODUCT('Bearing riser','Bearing riser','Bearing riser',(#9405));
#9412=PRODUCT('Mounting bush','Mounting bush','Mounting bush',(#9405));
#9413=PRODUCT('Mounting bush (1)','Mounting bush (1)','Mounting bush (1)',(#9405));
#9414=PRODUCT('Bearing riser (1)','Bearing riser (1)','Bearing riser (1)',(#9405));
#9415=PRODUCT('Mounting bush (2)','Mounting bush (2)','Mounting bush (2)',(#9405));
#9416=PRODUCT('Mounting bush (3)','Mounting bush (3)','Mounting bush (3)',(#9405));
#9417=PRODUCT('Pillow Block Bearing - 20 mm Bore',
'Pillow Block Bearing - 20 mm Bore','Pillow Block Bearing - 20 mm Bore',
(#9405));
#9418=PRODUCT('Housing','Housing','Housing',(#9405));
#9419=PRODUCT('Insert bearing','Insert bearing','Insert bearing',(#9405));
#9420=PRODUCT('Flat Washer - M8','Flat Washer - M8','Flat Washer - M8',
(#9405));
#9421=PRODUCT('M8x25 Bolt','M8x25 Bolt','M8x25 Bolt',(#9405));
#9422=PRODUCT('Coupled shafts','Coupled shafts','Coupled shafts',(#9405));
#9423=PRODUCT('Shaft stub','Shaft stub','Shaft stub',(#9405));
#9424=PRODUCT('Flange A','Flange A','Flange A',(#9405));
#9425=PRODUCT('End keeper','End keeper','End keeper',(#9405));
#9426=PRODUCT('Shaft stub (1)','Shaft stub (1)','Shaft stub (1)',(#9405));
#9427=PRODUCT('Flange B','Flange B','Flange B',(#9405));
#9428=PRODUCT('End keeper (1)','End keeper (1)','End keeper (1)',(#9405));
#9429=PRODUCT('Pilot ring','Pilot ring','Pilot ring',(#9405));
#9430=PRODUCT('End collar','End collar','End collar',(#9405));
#9431=PRODUCT('End collar (1)','End collar (1)','End collar (1)',(#9405));
#9432=PRODUCT('Key 6x6x20','Key 6x6x20','Key 6x6x20',(#9405));
#9433=PRODUCT('Cap Screw - M5x20','Cap Screw - M5x20',
'Cap Screw - M5x20',(#9405));
#9434=PRODUCT('Cap Screw - M6x25','Cap Screw - M6x25',
'Cap Screw - M6x25',(#9405));
#9435=PRODUCT('Flat Washer - M6','Flat Washer - M6','Flat Washer - M6',
(#9405));
#9436=PRODUCT('Hex Nut - M6','Hex Nut - M6','Hex Nut - M6',(#9405));
#9437=PRODUCT('Socket Set Screw - M5x8','Socket Set Screw - M5x8',
'Socket Set Screw - M5x8',(#9405));
#9438=PRESENTATION_STYLE_ASSIGNMENT((#9443));
#9439=PRESENTATION_STYLE_ASSIGNMENT((#9444));
#9440=PRESENTATION_STYLE_ASSIGNMENT((#9445));
#9441=PRESENTATION_STYLE_ASSIGNMENT((#9446));
#9442=PRESENTATION_STYLE_ASSIGNMENT((#9447));
#9443=SURFACE_STYLE_USAGE(.BOTH.,#9448);
#9444=SURFACE_STYLE_USAGE(.BOTH.,#9449);
#9445=SURFACE_STYLE_USAGE(.BOTH.,#9450);
#9446=SURFACE_STYLE_USAGE(.BOTH.,#9451);
#9447=SURFACE_STYLE_USAGE(.BOTH.,#9452);
#9448=SURFACE_SIDE_STYLE('',(#9453));
#9449=SURFACE_SIDE_STYLE('',(#9454));
#9450=SURFACE_SIDE_STYLE('',(#9455));
#9451=SURFACE_SIDE_STYLE('',(#9456));
#9452=SURFACE_SIDE_STYLE('',(#9457));
#9453=SURFACE_STYLE_FILL_AREA(#9458);
#9454=SURFACE_STYLE_FILL_AREA(#9459);
#9455=SURFACE_STYLE_FILL_AREA(#9460);
#9456=SURFACE_STYLE_FILL_AREA(#9461);
#9457=SURFACE_STYLE_FILL_AREA(#9462);
#9458=FILL_AREA_STYLE('Steel - Satin',(#9463));
#9459=FILL_AREA_STYLE('CAD Library Painted - Deep blue',(#9464));
#9460=FILL_AREA_STYLE('CAD Library Painted - Graphite',(#9465));
#9461=FILL_AREA_STYLE('CAD Library Painted - Steel gray',(#9466));
#9462=FILL_AREA_STYLE('CAD Library Painted - Engineering blue',(#9467));
#9463=FILL_AREA_STYLE_COLOUR('Steel - Satin',#9468);
#9464=FILL_AREA_STYLE_COLOUR('CAD Library Painted - Deep blue',#9469);
#9465=FILL_AREA_STYLE_COLOUR('CAD Library Painted - Graphite',#9470);
#9466=FILL_AREA_STYLE_COLOUR('CAD Library Painted - Steel gray',#9471);
#9467=FILL_AREA_STYLE_COLOUR('CAD Library Painted - Engineering blue',#9472);
#9468=COLOUR_RGB('Steel - Satin',0.627450980392157,0.627450980392157,0.627450980392157);
#9469=COLOUR_RGB('CAD Library Painted - Deep blue',0.0784313725490196,0.203921568627451,
0.349019607843137);
#9470=COLOUR_RGB('CAD Library Painted - Graphite',0.168627450980392,0.192156862745098,
0.231372549019608);
#9471=COLOUR_RGB('CAD Library Painted - Steel gray',0.592156862745098,0.631372549019608,
0.67843137254902);
#9472=COLOUR_RGB('CAD Library Painted - Engineering blue',0.12156862745098,
0.356862745098039,0.6);
#9473=COLOUR_RGB('Dark Blue',0.08,0.2,0.34);
#9474=FILL_AREA_STYLE_COLOUR('',#9473);
#9475=FILL_AREA_STYLE('',(#9474));
#9476=SURFACE_STYLE_FILL_AREA(#9475);
#9477=SURFACE_SIDE_STYLE('',(#9476));
#9478=SURFACE_STYLE_USAGE(.BOTH.,#9477);
#9479=PRESENTATION_STYLE_ASSIGNMENT((#9478));
#9480=COLOUR_RGB('Light Blue',0.38,0.62,0.78);
#9481=FILL_AREA_STYLE_COLOUR('',#9480);
#9482=FILL_AREA_STYLE('',(#9481));
#9483=SURFACE_STYLE_FILL_AREA(#9482);
#9484=SURFACE_SIDE_STYLE('',(#9483));
#9485=SURFACE_STYLE_USAGE(.BOTH.,#9484);
#9486=PRESENTATION_STYLE_ASSIGNMENT((#9485));
#9487=COLOUR_RGB('Sky Blue',0.24,0.69,0.87);
#9488=FILL_AREA_STYLE_COLOUR('',#9487);
#9489=FILL_AREA_STYLE('',(#9488));
#9490=SURFACE_STYLE_FILL_AREA(#9489);
#9491=SURFACE_SIDE_STYLE('',(#9490));
#9492=SURFACE_STYLE_USAGE(.BOTH.,#9491);
#9493=PRESENTATION_STYLE_ASSIGNMENT((#9492));
#9494=COLOUR_RGB('Grey',0.48,0.52,0.57);
#9495=FILL_AREA_STYLE_COLOUR('',#9494);
#9496=FILL_AREA_STYLE('',(#9495));
#9497=SURFACE_STYLE_FILL_AREA(#9496);
#9498=SURFACE_SIDE_STYLE('',(#9497));
#9499=SURFACE_STYLE_USAGE(.BOTH.,#9498);
#9500=PRESENTATION_STYLE_ASSIGNMENT((#9499));
#9501=COLOUR_RGB('Black',0.12,0.14,0.17);
#9502=FILL_AREA_STYLE_COLOUR('',#9501);
#9503=FILL_AREA_STYLE('',(#9502));
#9504=SURFACE_STYLE_FILL_AREA(#9503);
#9505=SURFACE_SIDE_STYLE('',(#9504));
#9506=SURFACE_STYLE_USAGE(.BOTH.,#9505);
#9507=PRESENTATION_STYLE_ASSIGNMENT((#9506));
#9508=COLOUR_RGB('Off White',0.89,0.88,0.83);
#9509=FILL_AREA_STYLE_COLOUR('',#9508);
#9510=FILL_AREA_STYLE('',(#9509));
#9511=SURFACE_STYLE_FILL_AREA(#9510);
#9512=SURFACE_SIDE_STYLE('',(#9511));
#9513=SURFACE_STYLE_USAGE(.BOTH.,#9512);
#9514=PRESENTATION_STYLE_ASSIGNMENT((#9513));
ENDSEC;
END-ISO-10303-21;
